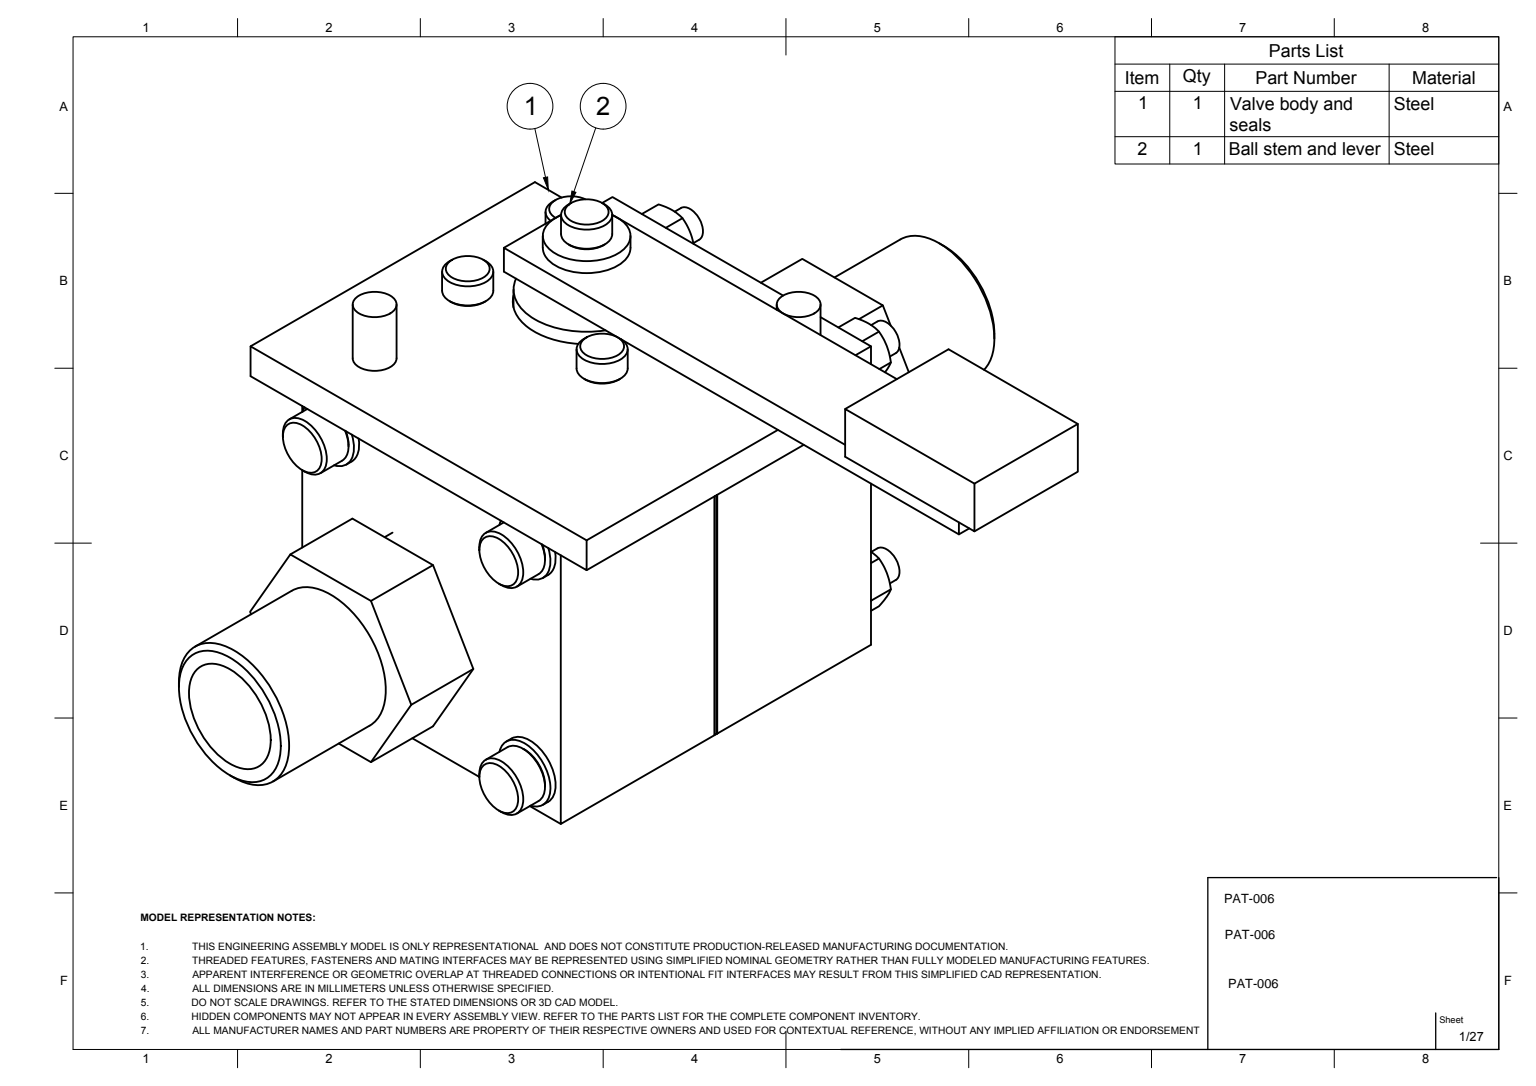
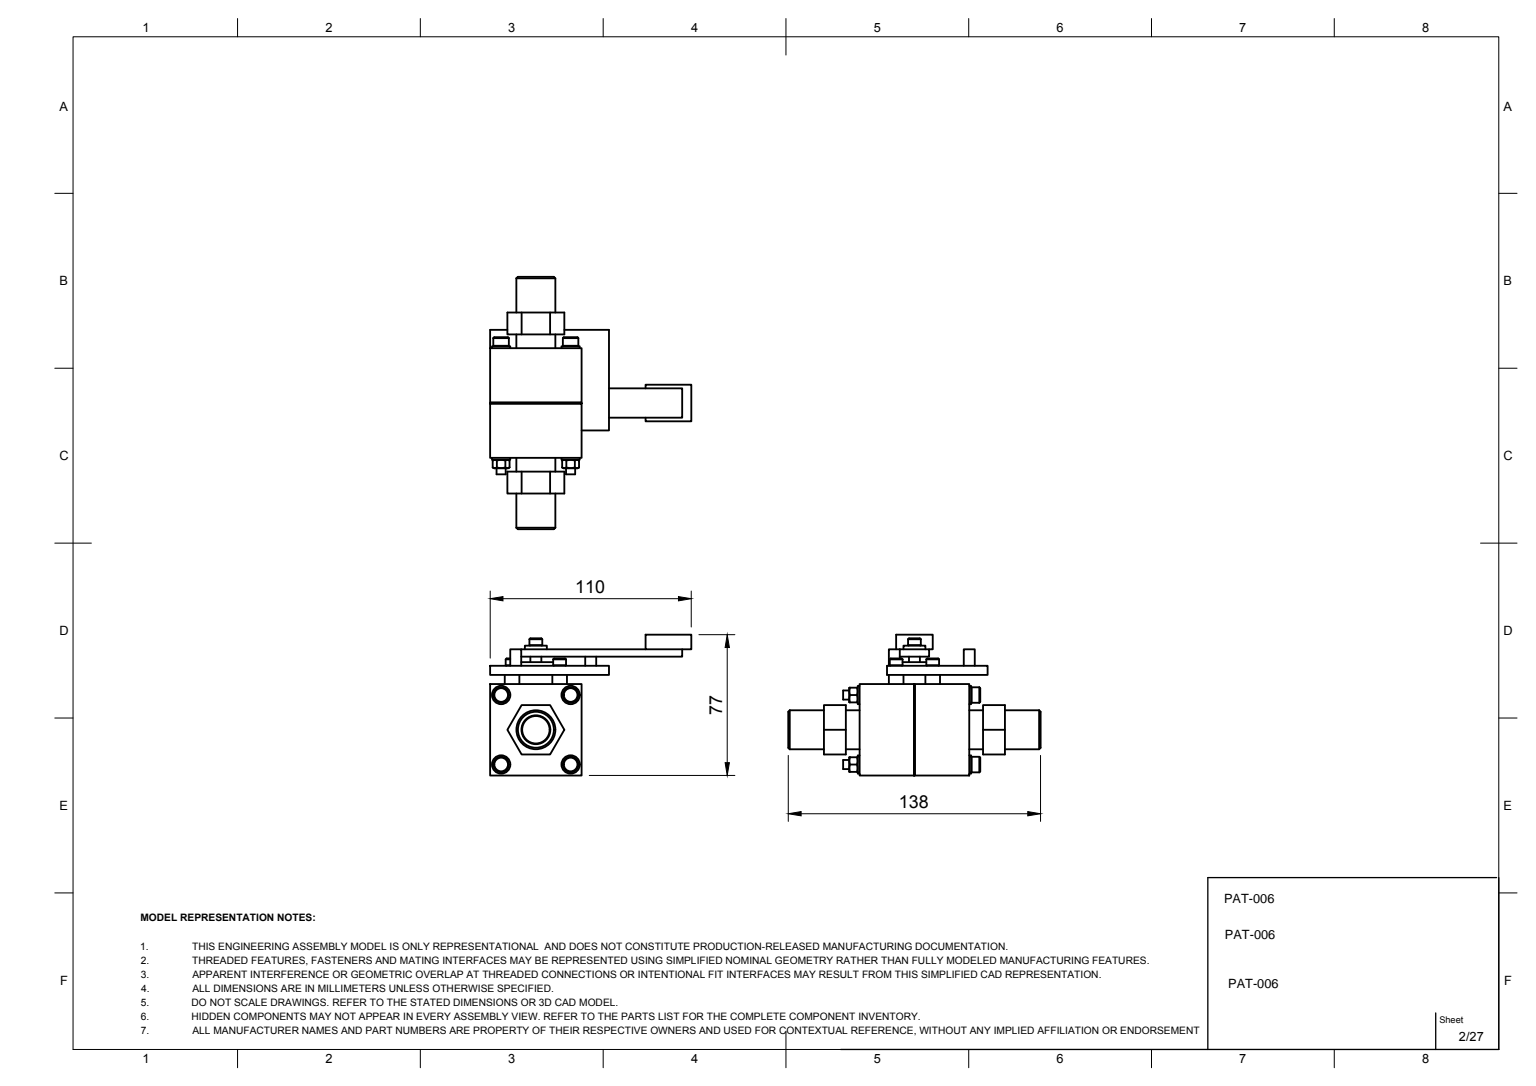
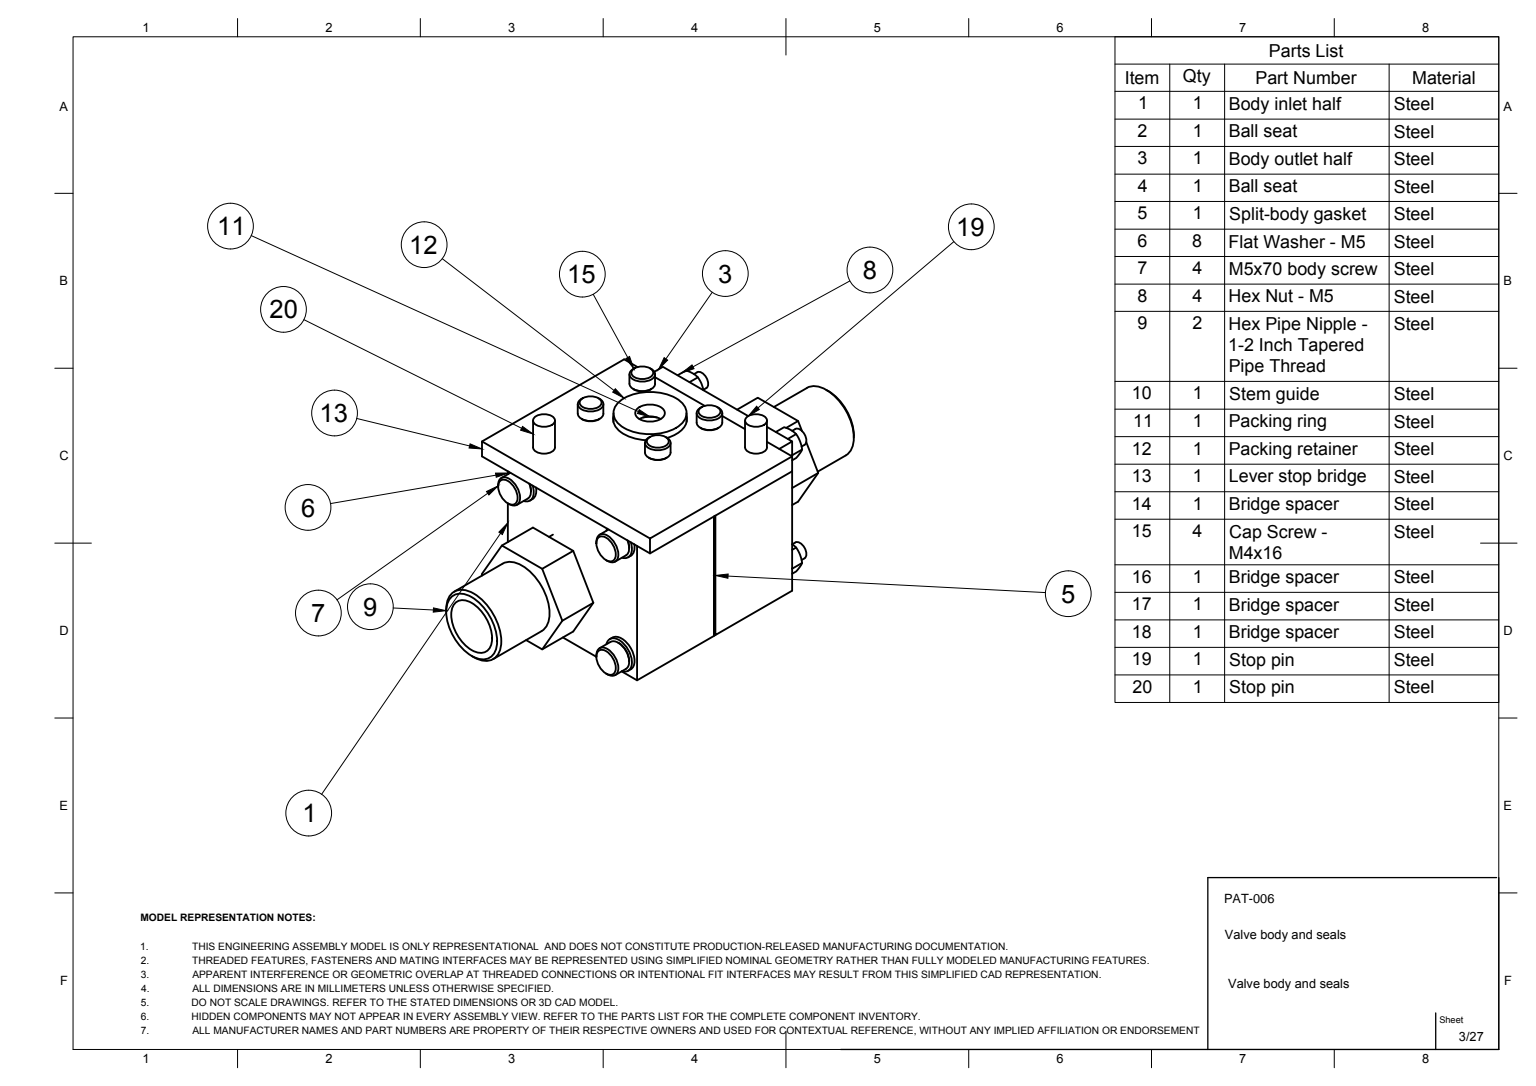
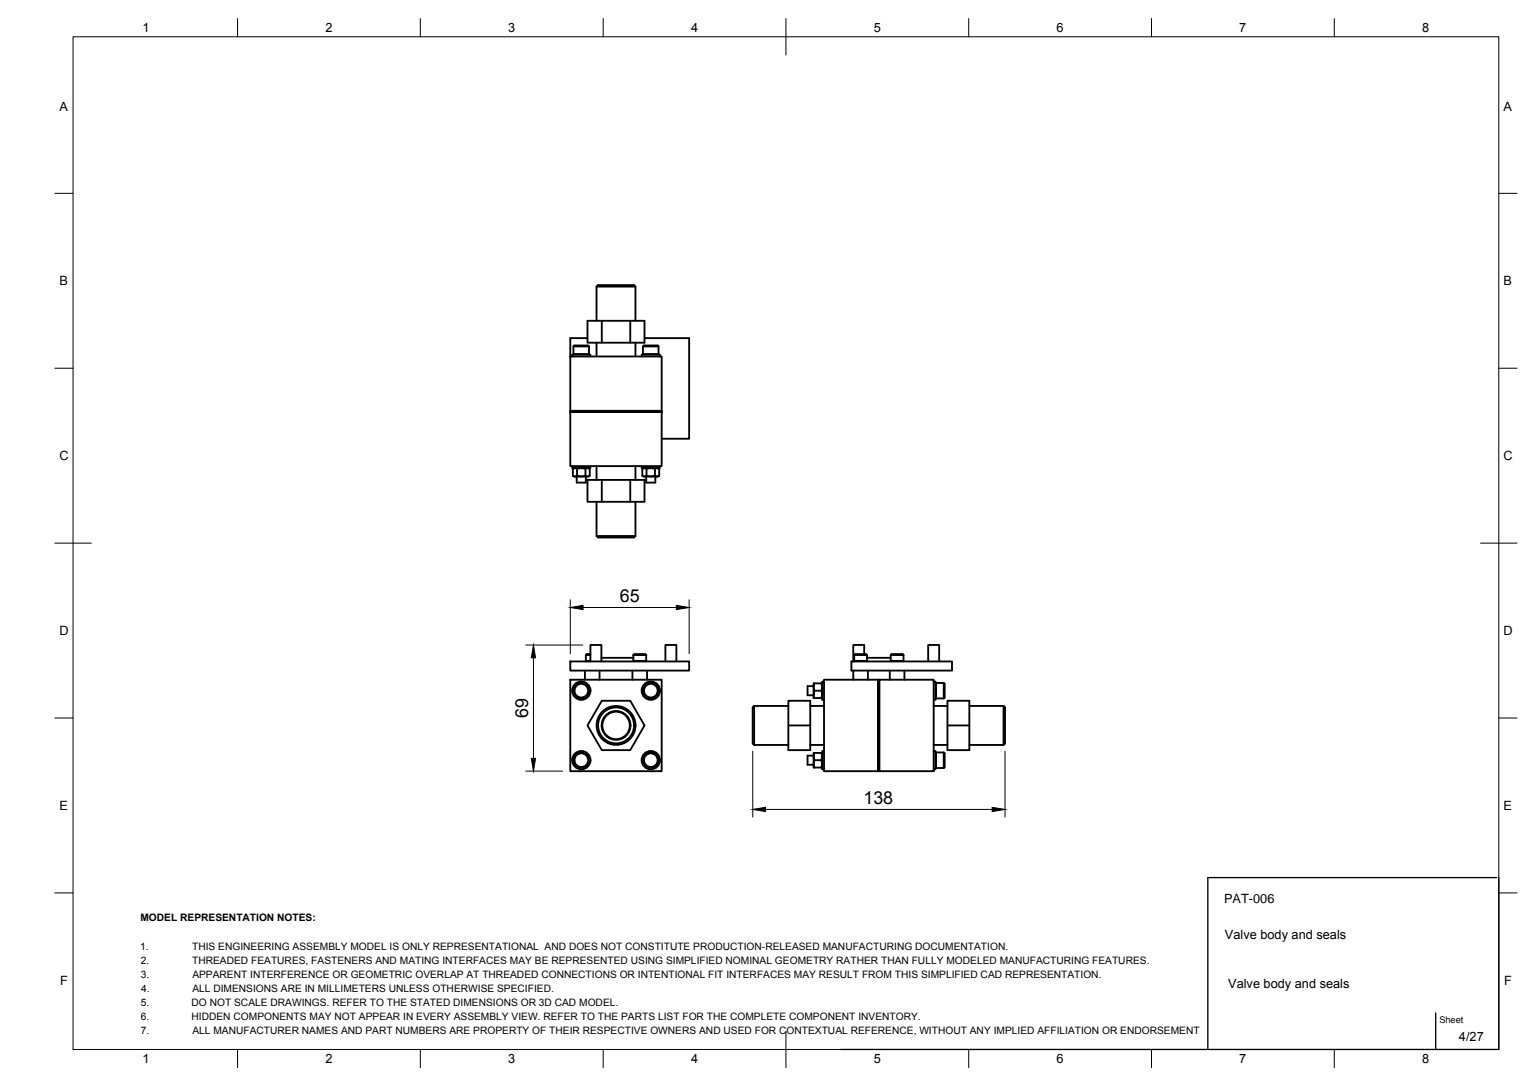
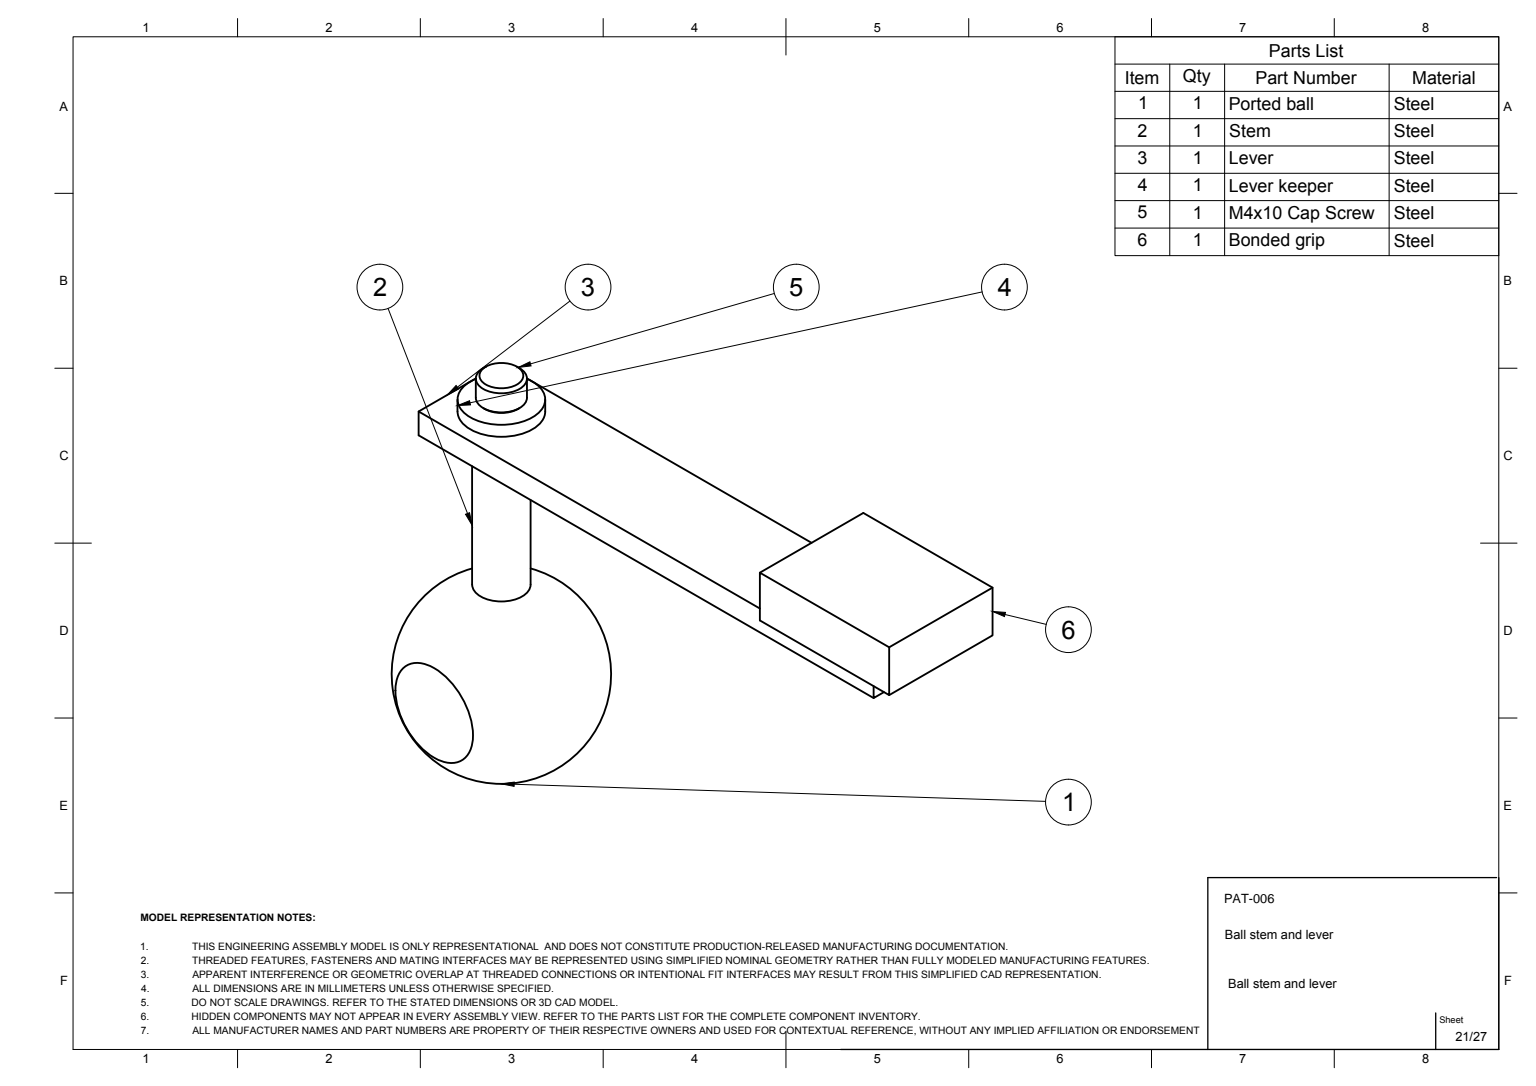
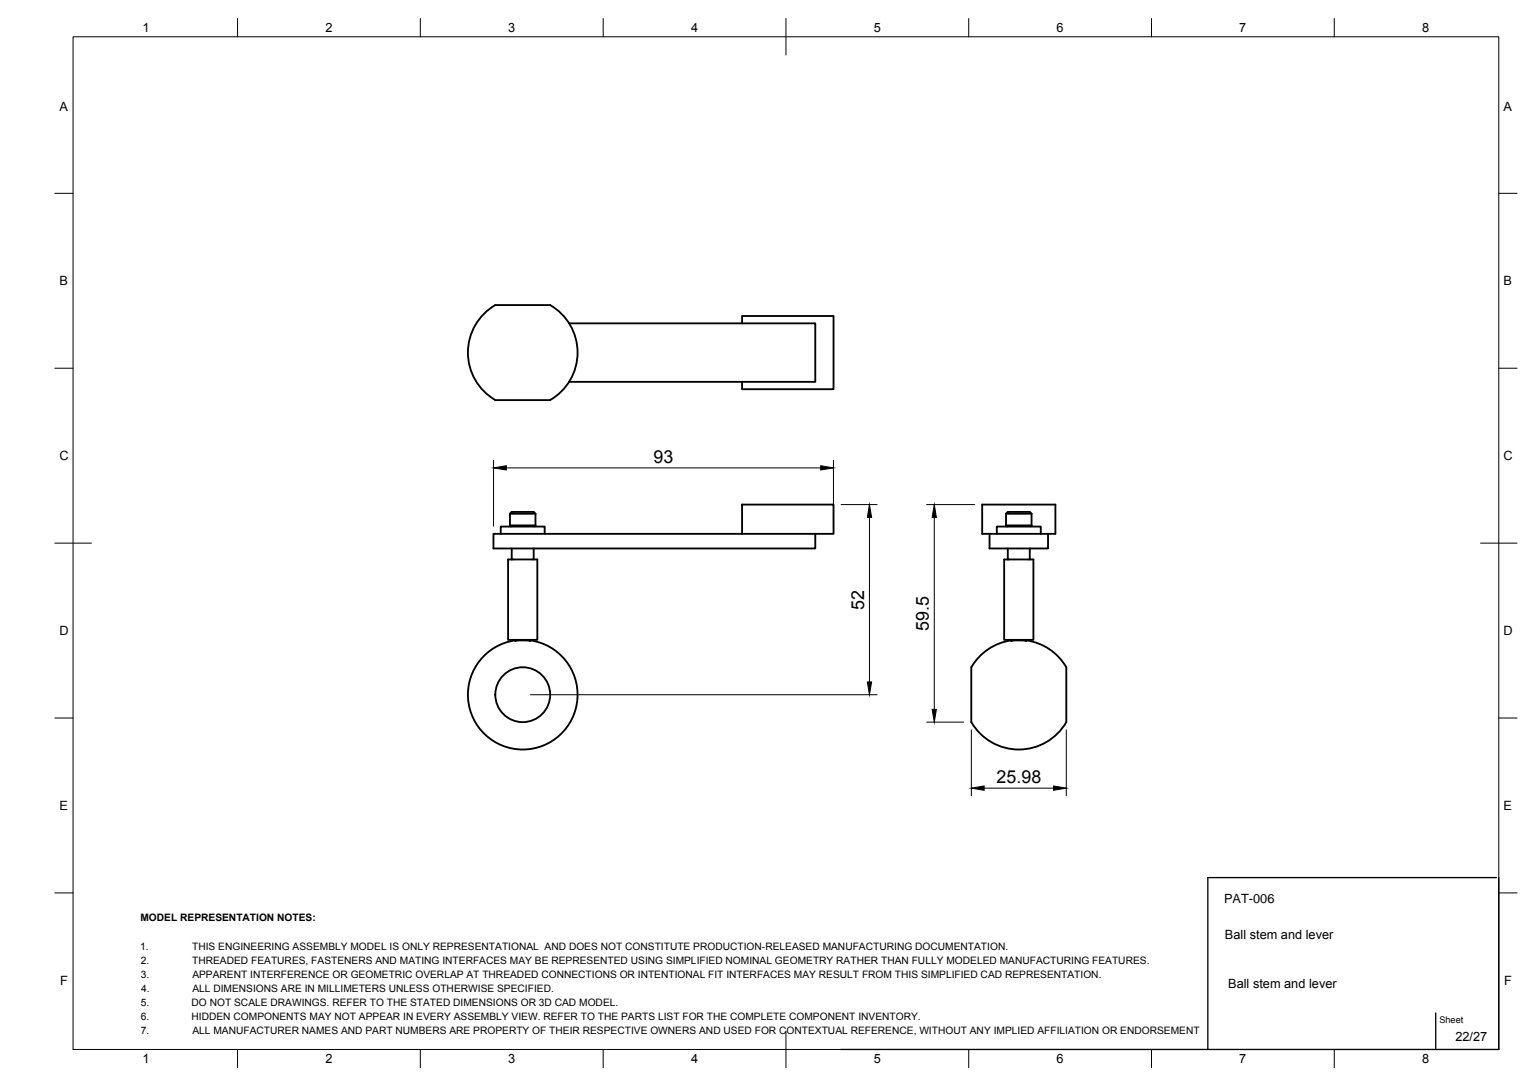
ISO-10303-21;
HEADER;
/* Generated by software containing ST-Developer
 * from STEP Tools, Inc. (www.steptools.com) 
 */

FILE_DESCRIPTION(
/* description */ ('Ball-type isolation valve (generic)'),
/* implementation_level */ '2;1');

FILE_NAME(
/* name */ 'PAT-006',
/* time_stamp */ '2026-10-27T10:53:05-07:00',
/* author */ (''),
/* organization */ (''),
/* preprocessor_version */ 'ST-DEVELOPER v20.2',
/* originating_system */ 'Autodesk Translation Framework v15.17.0.0',
/* authorisation */ '');

FILE_SCHEMA (('AUTOMOTIVE_DESIGN { 1 0 10303 214 3 1 1 }'));
ENDSEC;

DATA;
#10=MECHANICAL_DESIGN_GEOMETRIC_PRESENTATION_REPRESENTATION('',(#277,#278,
#279,#280,#281,#282,#283,#284,#285,#286,#287,#288,#289,#290,#291,#292,#293,
#294,#295,#296,#297,#298,#299,#300,#301,#302),#7425);
#11=ITEM_DEFINED_TRANSFORMATION($,$,#4400,#4748);
#12=ITEM_DEFINED_TRANSFORMATION($,$,#4443,#4749);
#13=ITEM_DEFINED_TRANSFORMATION($,$,#4454,#4750);
#14=ITEM_DEFINED_TRANSFORMATION($,$,#4497,#4751);
#15=ITEM_DEFINED_TRANSFORMATION($,$,#4508,#4752);
#16=ITEM_DEFINED_TRANSFORMATION($,$,#4535,#4753);
#17=ITEM_DEFINED_TRANSFORMATION($,$,#4548,#4754);
#18=ITEM_DEFINED_TRANSFORMATION($,$,#4552,#4755);
#19=ITEM_DEFINED_TRANSFORMATION($,$,#4565,#4756);
#20=ITEM_DEFINED_TRANSFORMATION($,$,#4595,#4757);
#21=ITEM_DEFINED_TRANSFORMATION($,$,#4604,#4758);
#22=ITEM_DEFINED_TRANSFORMATION($,$,#4613,#4759);
#23=ITEM_DEFINED_TRANSFORMATION($,$,#4622,#4760);
#24=ITEM_DEFINED_TRANSFORMATION($,$,#4631,#4761);
#25=ITEM_DEFINED_TRANSFORMATION($,$,#4637,#4762);
#26=ITEM_DEFINED_TRANSFORMATION($,$,#4671,#4763);
#27=ITEM_DEFINED_TRANSFORMATION($,$,#4643,#4764);
#28=ITEM_DEFINED_TRANSFORMATION($,$,#4671,#4765);
#29=ITEM_DEFINED_TRANSFORMATION($,$,#4682,#4766);
#30=ITEM_DEFINED_TRANSFORMATION($,$,#4671,#4767);
#31=ITEM_DEFINED_TRANSFORMATION($,$,#4643,#4768);
#32=ITEM_DEFINED_TRANSFORMATION($,$,#4671,#4769);
#33=ITEM_DEFINED_TRANSFORMATION($,$,#4682,#4770);
#34=ITEM_DEFINED_TRANSFORMATION($,$,#4671,#4771);
#35=ITEM_DEFINED_TRANSFORMATION($,$,#4643,#4772);
#36=ITEM_DEFINED_TRANSFORMATION($,$,#4671,#4773);
#37=ITEM_DEFINED_TRANSFORMATION($,$,#4682,#4774);
#38=ITEM_DEFINED_TRANSFORMATION($,$,#4671,#4775);
#39=ITEM_DEFINED_TRANSFORMATION($,$,#4643,#4776);
#40=ITEM_DEFINED_TRANSFORMATION($,$,#4671,#4777);
#41=ITEM_DEFINED_TRANSFORMATION($,$,#4682,#4778);
#42=ITEM_DEFINED_TRANSFORMATION($,$,#4698,#4779);
#43=ITEM_DEFINED_TRANSFORMATION($,$,#4698,#4780);
#44=ITEM_DEFINED_TRANSFORMATION($,$,#4722,#4781);
#45=ITEM_DEFINED_TRANSFORMATION($,$,#4722,#4782);
#46=ITEM_DEFINED_TRANSFORMATION($,$,#4722,#4783);
#47=ITEM_DEFINED_TRANSFORMATION($,$,#4722,#4784);
#48=ITEM_DEFINED_TRANSFORMATION($,$,#4786,#4888);
#49=ITEM_DEFINED_TRANSFORMATION($,$,#4802,#4889);
#50=ITEM_DEFINED_TRANSFORMATION($,$,#4837,#4890);
#51=ITEM_DEFINED_TRANSFORMATION($,$,#4848,#4891);
#52=ITEM_DEFINED_TRANSFORMATION($,$,#4857,#4892);
#53=ITEM_DEFINED_TRANSFORMATION($,$,#4864,#4893);
#54=ITEM_DEFINED_TRANSFORMATION($,$,#4399,#4894);
#55=ITEM_DEFINED_TRANSFORMATION($,$,#4785,#4895);
#56=(
REPRESENTATION_RELATIONSHIP($,$,#7535,#7534)
REPRESENTATION_RELATIONSHIP_WITH_TRANSFORMATION(#11)
SHAPE_REPRESENTATION_RELATIONSHIP()
);
#57=(
REPRESENTATION_RELATIONSHIP($,$,#7536,#7534)
REPRESENTATION_RELATIONSHIP_WITH_TRANSFORMATION(#12)
SHAPE_REPRESENTATION_RELATIONSHIP()
);
#58=(
REPRESENTATION_RELATIONSHIP($,$,#7537,#7534)
REPRESENTATION_RELATIONSHIP_WITH_TRANSFORMATION(#13)
SHAPE_REPRESENTATION_RELATIONSHIP()
);
#59=(
REPRESENTATION_RELATIONSHIP($,$,#7538,#7534)
REPRESENTATION_RELATIONSHIP_WITH_TRANSFORMATION(#14)
SHAPE_REPRESENTATION_RELATIONSHIP()
);
#60=(
REPRESENTATION_RELATIONSHIP($,$,#7539,#7534)
REPRESENTATION_RELATIONSHIP_WITH_TRANSFORMATION(#15)
SHAPE_REPRESENTATION_RELATIONSHIP()
);
#61=(
REPRESENTATION_RELATIONSHIP($,$,#7540,#7534)
REPRESENTATION_RELATIONSHIP_WITH_TRANSFORMATION(#16)
SHAPE_REPRESENTATION_RELATIONSHIP()
);
#62=(
REPRESENTATION_RELATIONSHIP($,$,#7541,#7534)
REPRESENTATION_RELATIONSHIP_WITH_TRANSFORMATION(#17)
SHAPE_REPRESENTATION_RELATIONSHIP()
);
#63=(
REPRESENTATION_RELATIONSHIP($,$,#7542,#7534)
REPRESENTATION_RELATIONSHIP_WITH_TRANSFORMATION(#18)
SHAPE_REPRESENTATION_RELATIONSHIP()
);
#64=(
REPRESENTATION_RELATIONSHIP($,$,#7543,#7534)
REPRESENTATION_RELATIONSHIP_WITH_TRANSFORMATION(#19)
SHAPE_REPRESENTATION_RELATIONSHIP()
);
#65=(
REPRESENTATION_RELATIONSHIP($,$,#7544,#7534)
REPRESENTATION_RELATIONSHIP_WITH_TRANSFORMATION(#20)
SHAPE_REPRESENTATION_RELATIONSHIP()
);
#66=(
REPRESENTATION_RELATIONSHIP($,$,#7545,#7534)
REPRESENTATION_RELATIONSHIP_WITH_TRANSFORMATION(#21)
SHAPE_REPRESENTATION_RELATIONSHIP()
);
#67=(
REPRESENTATION_RELATIONSHIP($,$,#7546,#7534)
REPRESENTATION_RELATIONSHIP_WITH_TRANSFORMATION(#22)
SHAPE_REPRESENTATION_RELATIONSHIP()
);
#68=(
REPRESENTATION_RELATIONSHIP($,$,#7547,#7534)
REPRESENTATION_RELATIONSHIP_WITH_TRANSFORMATION(#23)
SHAPE_REPRESENTATION_RELATIONSHIP()
);
#69=(
REPRESENTATION_RELATIONSHIP($,$,#7548,#7534)
REPRESENTATION_RELATIONSHIP_WITH_TRANSFORMATION(#24)
SHAPE_REPRESENTATION_RELATIONSHIP()
);
#70=(
REPRESENTATION_RELATIONSHIP($,$,#7549,#7534)
REPRESENTATION_RELATIONSHIP_WITH_TRANSFORMATION(#25)
SHAPE_REPRESENTATION_RELATIONSHIP()
);
#71=(
REPRESENTATION_RELATIONSHIP($,$,#7551,#7534)
REPRESENTATION_RELATIONSHIP_WITH_TRANSFORMATION(#26)
SHAPE_REPRESENTATION_RELATIONSHIP()
);
#72=(
REPRESENTATION_RELATIONSHIP($,$,#7550,#7534)
REPRESENTATION_RELATIONSHIP_WITH_TRANSFORMATION(#27)
SHAPE_REPRESENTATION_RELATIONSHIP()
);
#73=(
REPRESENTATION_RELATIONSHIP($,$,#7551,#7534)
REPRESENTATION_RELATIONSHIP_WITH_TRANSFORMATION(#28)
SHAPE_REPRESENTATION_RELATIONSHIP()
);
#74=(
REPRESENTATION_RELATIONSHIP($,$,#7552,#7534)
REPRESENTATION_RELATIONSHIP_WITH_TRANSFORMATION(#29)
SHAPE_REPRESENTATION_RELATIONSHIP()
);
#75=(
REPRESENTATION_RELATIONSHIP($,$,#7551,#7534)
REPRESENTATION_RELATIONSHIP_WITH_TRANSFORMATION(#30)
SHAPE_REPRESENTATION_RELATIONSHIP()
);
#76=(
REPRESENTATION_RELATIONSHIP($,$,#7550,#7534)
REPRESENTATION_RELATIONSHIP_WITH_TRANSFORMATION(#31)
SHAPE_REPRESENTATION_RELATIONSHIP()
);
#77=(
REPRESENTATION_RELATIONSHIP($,$,#7551,#7534)
REPRESENTATION_RELATIONSHIP_WITH_TRANSFORMATION(#32)
SHAPE_REPRESENTATION_RELATIONSHIP()
);
#78=(
REPRESENTATION_RELATIONSHIP($,$,#7552,#7534)
REPRESENTATION_RELATIONSHIP_WITH_TRANSFORMATION(#33)
SHAPE_REPRESENTATION_RELATIONSHIP()
);
#79=(
REPRESENTATION_RELATIONSHIP($,$,#7551,#7534)
REPRESENTATION_RELATIONSHIP_WITH_TRANSFORMATION(#34)
SHAPE_REPRESENTATION_RELATIONSHIP()
);
#80=(
REPRESENTATION_RELATIONSHIP($,$,#7550,#7534)
REPRESENTATION_RELATIONSHIP_WITH_TRANSFORMATION(#35)
SHAPE_REPRESENTATION_RELATIONSHIP()
);
#81=(
REPRESENTATION_RELATIONSHIP($,$,#7551,#7534)
REPRESENTATION_RELATIONSHIP_WITH_TRANSFORMATION(#36)
SHAPE_REPRESENTATION_RELATIONSHIP()
);
#82=(
REPRESENTATION_RELATIONSHIP($,$,#7552,#7534)
REPRESENTATION_RELATIONSHIP_WITH_TRANSFORMATION(#37)
SHAPE_REPRESENTATION_RELATIONSHIP()
);
#83=(
REPRESENTATION_RELATIONSHIP($,$,#7551,#7534)
REPRESENTATION_RELATIONSHIP_WITH_TRANSFORMATION(#38)
SHAPE_REPRESENTATION_RELATIONSHIP()
);
#84=(
REPRESENTATION_RELATIONSHIP($,$,#7550,#7534)
REPRESENTATION_RELATIONSHIP_WITH_TRANSFORMATION(#39)
SHAPE_REPRESENTATION_RELATIONSHIP()
);
#85=(
REPRESENTATION_RELATIONSHIP($,$,#7551,#7534)
REPRESENTATION_RELATIONSHIP_WITH_TRANSFORMATION(#40)
SHAPE_REPRESENTATION_RELATIONSHIP()
);
#86=(
REPRESENTATION_RELATIONSHIP($,$,#7552,#7534)
REPRESENTATION_RELATIONSHIP_WITH_TRANSFORMATION(#41)
SHAPE_REPRESENTATION_RELATIONSHIP()
);
#87=(
REPRESENTATION_RELATIONSHIP($,$,#7553,#7534)
REPRESENTATION_RELATIONSHIP_WITH_TRANSFORMATION(#42)
SHAPE_REPRESENTATION_RELATIONSHIP()
);
#88=(
REPRESENTATION_RELATIONSHIP($,$,#7553,#7534)
REPRESENTATION_RELATIONSHIP_WITH_TRANSFORMATION(#43)
SHAPE_REPRESENTATION_RELATIONSHIP()
);
#89=(
REPRESENTATION_RELATIONSHIP($,$,#7554,#7534)
REPRESENTATION_RELATIONSHIP_WITH_TRANSFORMATION(#44)
SHAPE_REPRESENTATION_RELATIONSHIP()
);
#90=(
REPRESENTATION_RELATIONSHIP($,$,#7554,#7534)
REPRESENTATION_RELATIONSHIP_WITH_TRANSFORMATION(#45)
SHAPE_REPRESENTATION_RELATIONSHIP()
);
#91=(
REPRESENTATION_RELATIONSHIP($,$,#7554,#7534)
REPRESENTATION_RELATIONSHIP_WITH_TRANSFORMATION(#46)
SHAPE_REPRESENTATION_RELATIONSHIP()
);
#92=(
REPRESENTATION_RELATIONSHIP($,$,#7554,#7534)
REPRESENTATION_RELATIONSHIP_WITH_TRANSFORMATION(#47)
SHAPE_REPRESENTATION_RELATIONSHIP()
);
#93=(
REPRESENTATION_RELATIONSHIP($,$,#7556,#7555)
REPRESENTATION_RELATIONSHIP_WITH_TRANSFORMATION(#48)
SHAPE_REPRESENTATION_RELATIONSHIP()
);
#94=(
REPRESENTATION_RELATIONSHIP($,$,#7557,#7555)
REPRESENTATION_RELATIONSHIP_WITH_TRANSFORMATION(#49)
SHAPE_REPRESENTATION_RELATIONSHIP()
);
#95=(
REPRESENTATION_RELATIONSHIP($,$,#7558,#7555)
REPRESENTATION_RELATIONSHIP_WITH_TRANSFORMATION(#50)
SHAPE_REPRESENTATION_RELATIONSHIP()
);
#96=(
REPRESENTATION_RELATIONSHIP($,$,#7559,#7555)
REPRESENTATION_RELATIONSHIP_WITH_TRANSFORMATION(#51)
SHAPE_REPRESENTATION_RELATIONSHIP()
);
#97=(
REPRESENTATION_RELATIONSHIP($,$,#7560,#7555)
REPRESENTATION_RELATIONSHIP_WITH_TRANSFORMATION(#52)
SHAPE_REPRESENTATION_RELATIONSHIP()
);
#98=(
REPRESENTATION_RELATIONSHIP($,$,#7561,#7555)
REPRESENTATION_RELATIONSHIP_WITH_TRANSFORMATION(#53)
SHAPE_REPRESENTATION_RELATIONSHIP()
);
#99=(
REPRESENTATION_RELATIONSHIP($,$,#7534,#7533)
REPRESENTATION_RELATIONSHIP_WITH_TRANSFORMATION(#54)
SHAPE_REPRESENTATION_RELATIONSHIP()
);
#100=(
REPRESENTATION_RELATIONSHIP($,$,#7555,#7533)
REPRESENTATION_RELATIONSHIP_WITH_TRANSFORMATION(#55)
SHAPE_REPRESENTATION_RELATIONSHIP()
);
#101=CONTEXT_DEPENDENT_SHAPE_REPRESENTATION(#56,#7481);
#102=CONTEXT_DEPENDENT_SHAPE_REPRESENTATION(#57,#7482);
#103=CONTEXT_DEPENDENT_SHAPE_REPRESENTATION(#58,#7483);
#104=CONTEXT_DEPENDENT_SHAPE_REPRESENTATION(#59,#7484);
#105=CONTEXT_DEPENDENT_SHAPE_REPRESENTATION(#60,#7485);
#106=CONTEXT_DEPENDENT_SHAPE_REPRESENTATION(#61,#7486);
#107=CONTEXT_DEPENDENT_SHAPE_REPRESENTATION(#62,#7487);
#108=CONTEXT_DEPENDENT_SHAPE_REPRESENTATION(#63,#7488);
#109=CONTEXT_DEPENDENT_SHAPE_REPRESENTATION(#64,#7489);
#110=CONTEXT_DEPENDENT_SHAPE_REPRESENTATION(#65,#7490);
#111=CONTEXT_DEPENDENT_SHAPE_REPRESENTATION(#66,#7491);
#112=CONTEXT_DEPENDENT_SHAPE_REPRESENTATION(#67,#7492);
#113=CONTEXT_DEPENDENT_SHAPE_REPRESENTATION(#68,#7493);
#114=CONTEXT_DEPENDENT_SHAPE_REPRESENTATION(#69,#7494);
#115=CONTEXT_DEPENDENT_SHAPE_REPRESENTATION(#70,#7495);
#116=CONTEXT_DEPENDENT_SHAPE_REPRESENTATION(#71,#7496);
#117=CONTEXT_DEPENDENT_SHAPE_REPRESENTATION(#72,#7497);
#118=CONTEXT_DEPENDENT_SHAPE_REPRESENTATION(#73,#7498);
#119=CONTEXT_DEPENDENT_SHAPE_REPRESENTATION(#74,#7499);
#120=CONTEXT_DEPENDENT_SHAPE_REPRESENTATION(#75,#7500);
#121=CONTEXT_DEPENDENT_SHAPE_REPRESENTATION(#76,#7501);
#122=CONTEXT_DEPENDENT_SHAPE_REPRESENTATION(#77,#7502);
#123=CONTEXT_DEPENDENT_SHAPE_REPRESENTATION(#78,#7503);
#124=CONTEXT_DEPENDENT_SHAPE_REPRESENTATION(#79,#7504);
#125=CONTEXT_DEPENDENT_SHAPE_REPRESENTATION(#80,#7505);
#126=CONTEXT_DEPENDENT_SHAPE_REPRESENTATION(#81,#7506);
#127=CONTEXT_DEPENDENT_SHAPE_REPRESENTATION(#82,#7507);
#128=CONTEXT_DEPENDENT_SHAPE_REPRESENTATION(#83,#7508);
#129=CONTEXT_DEPENDENT_SHAPE_REPRESENTATION(#84,#7509);
#130=CONTEXT_DEPENDENT_SHAPE_REPRESENTATION(#85,#7510);
#131=CONTEXT_DEPENDENT_SHAPE_REPRESENTATION(#86,#7511);
#132=CONTEXT_DEPENDENT_SHAPE_REPRESENTATION(#87,#7512);
#133=CONTEXT_DEPENDENT_SHAPE_REPRESENTATION(#88,#7513);
#134=CONTEXT_DEPENDENT_SHAPE_REPRESENTATION(#89,#7514);
#135=CONTEXT_DEPENDENT_SHAPE_REPRESENTATION(#90,#7515);
#136=CONTEXT_DEPENDENT_SHAPE_REPRESENTATION(#91,#7516);
#137=CONTEXT_DEPENDENT_SHAPE_REPRESENTATION(#92,#7517);
#138=CONTEXT_DEPENDENT_SHAPE_REPRESENTATION(#93,#7525);
#139=CONTEXT_DEPENDENT_SHAPE_REPRESENTATION(#94,#7526);
#140=CONTEXT_DEPENDENT_SHAPE_REPRESENTATION(#95,#7527);
#141=CONTEXT_DEPENDENT_SHAPE_REPRESENTATION(#96,#7528);
#142=CONTEXT_DEPENDENT_SHAPE_REPRESENTATION(#97,#7529);
#143=CONTEXT_DEPENDENT_SHAPE_REPRESENTATION(#98,#7530);
#144=CONTEXT_DEPENDENT_SHAPE_REPRESENTATION(#99,#7531);
#145=CONTEXT_DEPENDENT_SHAPE_REPRESENTATION(#100,#7532);
#146=NEXT_ASSEMBLY_USAGE_OCCURRENCE('Body inlet half:1',
'Body inlet half:1','Body inlet half:1',#7564,#7565,'Body inlet half:1');
#147=NEXT_ASSEMBLY_USAGE_OCCURRENCE('Ball seat:1','Ball seat:1',
'Ball seat:1',#7564,#7566,'Ball seat:1');
#148=NEXT_ASSEMBLY_USAGE_OCCURRENCE('Body outlet half:1',
'Body outlet half:1','Body outlet half:1',#7564,#7567,
'Body outlet half:1');
#149=NEXT_ASSEMBLY_USAGE_OCCURRENCE('Ball seat (1):1','Ball seat (1):1',
'Ball seat (1):1',#7564,#7568,'Ball seat (1):1');
#150=NEXT_ASSEMBLY_USAGE_OCCURRENCE('Split-body gasket:1',
'Split-body gasket:1','Split-body gasket:1',#7564,#7569,
'Split-body gasket:1');
#151=NEXT_ASSEMBLY_USAGE_OCCURRENCE('Stem guide:1','Stem guide:1',
'Stem guide:1',#7564,#7570,'Stem guide:1');
#152=NEXT_ASSEMBLY_USAGE_OCCURRENCE('Packing ring:1','Packing ring:1',
'Packing ring:1',#7564,#7571,'Packing ring:1');
#153=NEXT_ASSEMBLY_USAGE_OCCURRENCE('Packing retainer:1',
'Packing retainer:1','Packing retainer:1',#7564,#7572,
'Packing retainer:1');
#154=NEXT_ASSEMBLY_USAGE_OCCURRENCE('Lever stop bridge:1',
'Lever stop bridge:1','Lever stop bridge:1',#7564,#7573,
'Lever stop bridge:1');
#155=NEXT_ASSEMBLY_USAGE_OCCURRENCE('Bridge spacer:1','Bridge spacer:1',
'Bridge spacer:1',#7564,#7574,'Bridge spacer:1');
#156=NEXT_ASSEMBLY_USAGE_OCCURRENCE('Bridge spacer (1):1',
'Bridge spacer (1):1','Bridge spacer (1):1',#7564,#7575,
'Bridge spacer (1):1');
#157=NEXT_ASSEMBLY_USAGE_OCCURRENCE('Bridge spacer (2):1',
'Bridge spacer (2):1','Bridge spacer (2):1',#7564,#7576,
'Bridge spacer (2):1');
#158=NEXT_ASSEMBLY_USAGE_OCCURRENCE('Bridge spacer (3):1',
'Bridge spacer (3):1','Bridge spacer (3):1',#7564,#7577,
'Bridge spacer (3):1');
#159=NEXT_ASSEMBLY_USAGE_OCCURRENCE('Stop pin:1','Stop pin:1',
'Stop pin:1',#7564,#7578,'Stop pin:1');
#160=NEXT_ASSEMBLY_USAGE_OCCURRENCE('Stop pin (1):1','Stop pin (1):1',
'Stop pin (1):1',#7564,#7579,'Stop pin (1):1');
#161=NEXT_ASSEMBLY_USAGE_OCCURRENCE('Flat Washer - M5:2',
'Flat Washer - M5:2','Flat Washer - M5:2',#7564,#7581,
'Flat Washer - M5:2');
#162=NEXT_ASSEMBLY_USAGE_OCCURRENCE('M5x70 body screw:2',
'M5x70 body screw:2','M5x70 body screw:2',#7564,#7580,
'M5x70 body screw:2');
#163=NEXT_ASSEMBLY_USAGE_OCCURRENCE('Flat Washer - M5:3',
'Flat Washer - M5:3','Flat Washer - M5:3',#7564,#7581,
'Flat Washer - M5:3');
#164=NEXT_ASSEMBLY_USAGE_OCCURRENCE('Hex Nut - M5:2','Hex Nut - M5:2',
'Hex Nut - M5:2',#7564,#7582,'Hex Nut - M5:2');
#165=NEXT_ASSEMBLY_USAGE_OCCURRENCE('Flat Washer - M5:4',
'Flat Washer - M5:4','Flat Washer - M5:4',#7564,#7581,
'Flat Washer - M5:4');
#166=NEXT_ASSEMBLY_USAGE_OCCURRENCE('M5x70 body screw:3',
'M5x70 body screw:3','M5x70 body screw:3',#7564,#7580,
'M5x70 body screw:3');
#167=NEXT_ASSEMBLY_USAGE_OCCURRENCE('Flat Washer - M5:5',
'Flat Washer - M5:5','Flat Washer - M5:5',#7564,#7581,
'Flat Washer - M5:5');
#168=NEXT_ASSEMBLY_USAGE_OCCURRENCE('Hex Nut - M5:3','Hex Nut - M5:3',
'Hex Nut - M5:3',#7564,#7582,'Hex Nut - M5:3');
#169=NEXT_ASSEMBLY_USAGE_OCCURRENCE('Flat Washer - M5:6',
'Flat Washer - M5:6','Flat Washer - M5:6',#7564,#7581,
'Flat Washer - M5:6');
#170=NEXT_ASSEMBLY_USAGE_OCCURRENCE('M5x70 body screw:4',
'M5x70 body screw:4','M5x70 body screw:4',#7564,#7580,
'M5x70 body screw:4');
#171=NEXT_ASSEMBLY_USAGE_OCCURRENCE('Flat Washer - M5:7',
'Flat Washer - M5:7','Flat Washer - M5:7',#7564,#7581,
'Flat Washer - M5:7');
#172=NEXT_ASSEMBLY_USAGE_OCCURRENCE('Hex Nut - M5:4','Hex Nut - M5:4',
'Hex Nut - M5:4',#7564,#7582,'Hex Nut - M5:4');
#173=NEXT_ASSEMBLY_USAGE_OCCURRENCE('Flat Washer - M5:8',
'Flat Washer - M5:8','Flat Washer - M5:8',#7564,#7581,
'Flat Washer - M5:8');
#174=NEXT_ASSEMBLY_USAGE_OCCURRENCE('M5x70 body screw:5',
'M5x70 body screw:5','M5x70 body screw:5',#7564,#7580,
'M5x70 body screw:5');
#175=NEXT_ASSEMBLY_USAGE_OCCURRENCE('Flat Washer - M5:9',
'Flat Washer - M5:9','Flat Washer - M5:9',#7564,#7581,
'Flat Washer - M5:9');
#176=NEXT_ASSEMBLY_USAGE_OCCURRENCE('Hex Nut - M5:5','Hex Nut - M5:5',
'Hex Nut - M5:5',#7564,#7582,'Hex Nut - M5:5');
#177=NEXT_ASSEMBLY_USAGE_OCCURRENCE(
'Hex Pipe Nipple - 1-2 Inch Tapered Pipe Thread:2',
'Hex Pipe Nipple - 1-2 Inch Tapered Pipe Thread:2',
'Hex Pipe Nipple - 1-2 Inch Tapered Pipe Thread:2',#7564,#7583,
'Hex Pipe Nipple - 1-2 Inch Tapered Pipe Thread:2');
#178=NEXT_ASSEMBLY_USAGE_OCCURRENCE(
'Hex Pipe Nipple - 1-2 Inch Tapered Pipe Thread:3',
'Hex Pipe Nipple - 1-2 Inch Tapered Pipe Thread:3',
'Hex Pipe Nipple - 1-2 Inch Tapered Pipe Thread:3',#7564,#7583,
'Hex Pipe Nipple - 1-2 Inch Tapered Pipe Thread:3');
#179=NEXT_ASSEMBLY_USAGE_OCCURRENCE('Cap Screw - M4x16:2',
'Cap Screw - M4x16:2','Cap Screw - M4x16:2',#7564,#7584,
'Cap Screw - M4x16:2');
#180=NEXT_ASSEMBLY_USAGE_OCCURRENCE('Cap Screw - M4x16:3',
'Cap Screw - M4x16:3','Cap Screw - M4x16:3',#7564,#7584,
'Cap Screw - M4x16:3');
#181=NEXT_ASSEMBLY_USAGE_OCCURRENCE('Cap Screw - M4x16:4',
'Cap Screw - M4x16:4','Cap Screw - M4x16:4',#7564,#7584,
'Cap Screw - M4x16:4');
#182=NEXT_ASSEMBLY_USAGE_OCCURRENCE('Cap Screw - M4x16:5',
'Cap Screw - M4x16:5','Cap Screw - M4x16:5',#7564,#7584,
'Cap Screw - M4x16:5');
#183=NEXT_ASSEMBLY_USAGE_OCCURRENCE('Ported ball:1','Ported ball:1',
'Ported ball:1',#7585,#7586,'Ported ball:1');
#184=NEXT_ASSEMBLY_USAGE_OCCURRENCE('Stem:1','Stem:1','Stem:1',#7585,#7587,
'Stem:1');
#185=NEXT_ASSEMBLY_USAGE_OCCURRENCE('Lever:1','Lever:1','Lever:1',#7585,
#7588,'Lever:1');
#186=NEXT_ASSEMBLY_USAGE_OCCURRENCE('Lever keeper:1','Lever keeper:1',
'Lever keeper:1',#7585,#7589,'Lever keeper:1');
#187=NEXT_ASSEMBLY_USAGE_OCCURRENCE('Bonded grip:1','Bonded grip:1',
'Bonded grip:1',#7585,#7590,'Bonded grip:1');
#188=NEXT_ASSEMBLY_USAGE_OCCURRENCE('M4x10 Cap Screw:2',
'M4x10 Cap Screw:2','M4x10 Cap Screw:2',#7585,#7591,'M4x10 Cap Screw:2');
#189=NEXT_ASSEMBLY_USAGE_OCCURRENCE('Valve body and seals:1',
'Valve body and seals:1','Valve body and seals:1',#7563,#7564,
'Valve body and seals:1');
#190=NEXT_ASSEMBLY_USAGE_OCCURRENCE('Ball stem and lever:1',
'Ball stem and lever:1','Ball stem and lever:1',#7563,#7585,
'Ball stem and lever:1');
#191=(
BOUNDED_CURVE()
B_SPLINE_CURVE(2,(#6817,#6818,#6819),.UNSPECIFIED.,.F.,.F.)
B_SPLINE_CURVE_WITH_KNOTS((3,3),(0.140651836354967,0.670383167684795),
 .UNSPECIFIED.)
CURVE()
GEOMETRIC_REPRESENTATION_ITEM()
RATIONAL_B_SPLINE_CURVE((1.11602540378444,1.28867513459481,1.11602540378444))
REPRESENTATION_ITEM('')
);
#192=(
BOUNDED_CURVE()
B_SPLINE_CURVE(2,(#6821,#6822,#6823),.UNSPECIFIED.,.F.,.F.)
B_SPLINE_CURVE_WITH_KNOTS((3,3),(0.140651836354967,0.670383167684795),
 .UNSPECIFIED.)
CURVE()
GEOMETRIC_REPRESENTATION_ITEM()
RATIONAL_B_SPLINE_CURVE((1.11602540378444,1.28867513459481,1.11602540378444))
REPRESENTATION_ITEM('')
);
#193=(
BOUNDED_CURVE()
B_SPLINE_CURVE(2,(#6828,#6829,#6830),.UNSPECIFIED.,.F.,.F.)
B_SPLINE_CURVE_WITH_KNOTS((3,3),(0.140651836354967,0.670383167684795),
 .UNSPECIFIED.)
CURVE()
GEOMETRIC_REPRESENTATION_ITEM()
RATIONAL_B_SPLINE_CURVE((1.11602540378444,1.28867513459481,1.11602540378444))
REPRESENTATION_ITEM('')
);
#194=(
BOUNDED_CURVE()
B_SPLINE_CURVE(2,(#6832,#6833,#6834),.UNSPECIFIED.,.F.,.F.)
B_SPLINE_CURVE_WITH_KNOTS((3,3),(0.140651836354967,0.670383167684795),
 .UNSPECIFIED.)
CURVE()
GEOMETRIC_REPRESENTATION_ITEM()
RATIONAL_B_SPLINE_CURVE((1.11602540378444,1.28867513459481,1.11602540378444))
REPRESENTATION_ITEM('')
);
#195=(
BOUNDED_CURVE()
B_SPLINE_CURVE(2,(#6836,#6837,#6838),.UNSPECIFIED.,.F.,.F.)
B_SPLINE_CURVE_WITH_KNOTS((3,3),(0.140651836354967,0.670383167684795),
 .UNSPECIFIED.)
CURVE()
GEOMETRIC_REPRESENTATION_ITEM()
RATIONAL_B_SPLINE_CURVE((1.11602540378444,1.28867513459481,1.11602540378444))
REPRESENTATION_ITEM('')
);
#196=(
BOUNDED_CURVE()
B_SPLINE_CURVE(2,(#6839,#6840,#6841),.UNSPECIFIED.,.F.,.F.)
B_SPLINE_CURVE_WITH_KNOTS((3,3),(0.140651836354967,0.670383167684795),
 .UNSPECIFIED.)
CURVE()
GEOMETRIC_REPRESENTATION_ITEM()
RATIONAL_B_SPLINE_CURVE((1.11602540378444,1.28867513459481,1.11602540378444))
REPRESENTATION_ITEM('')
);
#197=(
BOUNDED_CURVE()
B_SPLINE_CURVE(2,(#6848,#6849,#6850),.UNSPECIFIED.,.F.,.F.)
B_SPLINE_CURVE_WITH_KNOTS((3,3),(0.140651836354967,0.670383167684795),
 .UNSPECIFIED.)
CURVE()
GEOMETRIC_REPRESENTATION_ITEM()
RATIONAL_B_SPLINE_CURVE((1.11602540378444,1.28867513459481,1.11602540378444))
REPRESENTATION_ITEM('')
);
#198=(
BOUNDED_CURVE()
B_SPLINE_CURVE(2,(#6852,#6853,#6854),.UNSPECIFIED.,.F.,.F.)
B_SPLINE_CURVE_WITH_KNOTS((3,3),(0.140651836354967,0.670383167684796),
 .UNSPECIFIED.)
CURVE()
GEOMETRIC_REPRESENTATION_ITEM()
RATIONAL_B_SPLINE_CURVE((1.11602540378444,1.28867513459481,1.11602540378444))
REPRESENTATION_ITEM('')
);
#199=(
BOUNDED_CURVE()
B_SPLINE_CURVE(2,(#6856,#6857,#6858),.UNSPECIFIED.,.F.,.F.)
B_SPLINE_CURVE_WITH_KNOTS((3,3),(0.140651836354967,0.670383167684795),
 .UNSPECIFIED.)
CURVE()
GEOMETRIC_REPRESENTATION_ITEM()
RATIONAL_B_SPLINE_CURVE((1.11602540378444,1.28867513459481,1.11602540378444))
REPRESENTATION_ITEM('')
);
#200=(
BOUNDED_CURVE()
B_SPLINE_CURVE(2,(#6860,#6861,#6862),.UNSPECIFIED.,.F.,.F.)
B_SPLINE_CURVE_WITH_KNOTS((3,3),(0.140651836354967,0.670383167684795),
 .UNSPECIFIED.)
CURVE()
GEOMETRIC_REPRESENTATION_ITEM()
RATIONAL_B_SPLINE_CURVE((1.11602540378444,1.28867513459482,1.11602540378444))
REPRESENTATION_ITEM('')
);
#201=(
BOUNDED_CURVE()
B_SPLINE_CURVE(2,(#6864,#6865,#6866),.UNSPECIFIED.,.F.,.F.)
B_SPLINE_CURVE_WITH_KNOTS((3,3),(0.140651836354967,0.670383167684795),
 .UNSPECIFIED.)
CURVE()
GEOMETRIC_REPRESENTATION_ITEM()
RATIONAL_B_SPLINE_CURVE((1.11602540378444,1.28867513459481,1.11602540378444))
REPRESENTATION_ITEM('')
);
#202=(
BOUNDED_CURVE()
B_SPLINE_CURVE(2,(#6867,#6868,#6869),.UNSPECIFIED.,.F.,.F.)
B_SPLINE_CURVE_WITH_KNOTS((3,3),(0.140651836354967,0.670383167684795),
 .UNSPECIFIED.)
CURVE()
GEOMETRIC_REPRESENTATION_ITEM()
RATIONAL_B_SPLINE_CURVE((1.11602540378444,1.28867513459481,1.11602540378444))
REPRESENTATION_ITEM('')
);
#203=CONICAL_SURFACE('',#4660,0.4,0.785398163397448);
#204=CONICAL_SURFACE('',#4664,0.41,0.785398163397448);
#205=CONICAL_SURFACE('',#4668,0.26,0.463647609000806);
#206=CONICAL_SURFACE('',#4672,0.275,0.785398163397449);
#207=CONICAL_SURFACE('',#4683,0.47094010767585,1.0471975511966);
#208=CONICAL_SURFACE('',#4685,0.47094010767585,1.0471975511966);
#209=CONICAL_SURFACE('',#4714,1.025,0.785398163397448);
#210=CONICAL_SURFACE('',#4717,1.025,0.785398163397448);
#211=CONICAL_SURFACE('',#4725,0.325,0.785398163397448);
#212=CONICAL_SURFACE('',#4729,0.335,0.785398163397448);
#213=CONICAL_SURFACE('',#4733,0.21,0.463647609000806);
#214=CONICAL_SURFACE('',#4737,0.18,0.785398163397448);
#215=CONICAL_SURFACE('',#4877,0.325,0.785398163397448);
#216=CONICAL_SURFACE('',#4881,0.335,0.785398163397448);
#217=CONICAL_SURFACE('',#4885,0.21,0.463647609000806);
#218=ORIENTED_CLOSED_SHELL('',*,#4097,.F.);
#219=ORIENTED_CLOSED_SHELL('',*,#4103,.F.);
#220=ORIENTED_CLOSED_SHELL('',*,#4109,.F.);
#221=BREP_WITH_VOIDS('Body1',#4098,(#218));
#222=BREP_WITH_VOIDS('Body1',#4102,(#219));
#223=BREP_WITH_VOIDS('Body1',#4110,(#220));
#224=TOROIDAL_SURFACE('',#4549,0.5,0.1);
#225=SHAPE_REPRESENTATION_RELATIONSHIP('SRR','None',#7535,#251);
#226=SHAPE_REPRESENTATION_RELATIONSHIP('SRR','None',#7536,#252);
#227=SHAPE_REPRESENTATION_RELATIONSHIP('SRR','None',#7537,#253);
#228=SHAPE_REPRESENTATION_RELATIONSHIP('SRR','None',#7538,#254);
#229=SHAPE_REPRESENTATION_RELATIONSHIP('SRR','None',#7539,#255);
#230=SHAPE_REPRESENTATION_RELATIONSHIP('SRR','None',#7540,#256);
#231=SHAPE_REPRESENTATION_RELATIONSHIP('SRR','None',#7541,#257);
#232=SHAPE_REPRESENTATION_RELATIONSHIP('SRR','None',#7542,#258);
#233=SHAPE_REPRESENTATION_RELATIONSHIP('SRR','None',#7543,#259);
#234=SHAPE_REPRESENTATION_RELATIONSHIP('SRR','None',#7544,#260);
#235=SHAPE_REPRESENTATION_RELATIONSHIP('SRR','None',#7545,#261);
#236=SHAPE_REPRESENTATION_RELATIONSHIP('SRR','None',#7546,#262);
#237=SHAPE_REPRESENTATION_RELATIONSHIP('SRR','None',#7547,#263);
#238=SHAPE_REPRESENTATION_RELATIONSHIP('SRR','None',#7548,#264);
#239=SHAPE_REPRESENTATION_RELATIONSHIP('SRR','None',#7549,#265);
#240=SHAPE_REPRESENTATION_RELATIONSHIP('SRR','None',#7550,#266);
#241=SHAPE_REPRESENTATION_RELATIONSHIP('SRR','None',#7551,#267);
#242=SHAPE_REPRESENTATION_RELATIONSHIP('SRR','None',#7552,#268);
#243=SHAPE_REPRESENTATION_RELATIONSHIP('SRR','None',#7553,#269);
#244=SHAPE_REPRESENTATION_RELATIONSHIP('SRR','None',#7554,#270);
#245=SHAPE_REPRESENTATION_RELATIONSHIP('SRR','None',#7556,#271);
#246=SHAPE_REPRESENTATION_RELATIONSHIP('SRR','None',#7557,#272);
#247=SHAPE_REPRESENTATION_RELATIONSHIP('SRR','None',#7558,#273);
#248=SHAPE_REPRESENTATION_RELATIONSHIP('SRR','None',#7559,#274);
#249=SHAPE_REPRESENTATION_RELATIONSHIP('SRR','None',#7560,#275);
#250=SHAPE_REPRESENTATION_RELATIONSHIP('SRR','None',#7561,#276);
#251=ADVANCED_BREP_SHAPE_REPRESENTATION('',(#303),#7398);
#252=ADVANCED_BREP_SHAPE_REPRESENTATION('',(#304),#7399);
#253=ADVANCED_BREP_SHAPE_REPRESENTATION('',(#305),#7400);
#254=ADVANCED_BREP_SHAPE_REPRESENTATION('',(#306),#7401);
#255=ADVANCED_BREP_SHAPE_REPRESENTATION('',(#307),#7402);
#256=ADVANCED_BREP_SHAPE_REPRESENTATION('',(#308),#7403);
#257=ADVANCED_BREP_SHAPE_REPRESENTATION('',(#309),#7404);
#258=ADVANCED_BREP_SHAPE_REPRESENTATION('',(#310),#7405);
#259=ADVANCED_BREP_SHAPE_REPRESENTATION('',(#311),#7406);
#260=ADVANCED_BREP_SHAPE_REPRESENTATION('',(#312),#7407);
#261=ADVANCED_BREP_SHAPE_REPRESENTATION('',(#313),#7408);
#262=ADVANCED_BREP_SHAPE_REPRESENTATION('',(#314),#7409);
#263=ADVANCED_BREP_SHAPE_REPRESENTATION('',(#315),#7410);
#264=ADVANCED_BREP_SHAPE_REPRESENTATION('',(#316),#7411);
#265=ADVANCED_BREP_SHAPE_REPRESENTATION('',(#317),#7412);
#266=ADVANCED_BREP_SHAPE_REPRESENTATION('',(#221),#7413);
#267=ADVANCED_BREP_SHAPE_REPRESENTATION('',(#318),#7414);
#268=ADVANCED_BREP_SHAPE_REPRESENTATION('',(#319),#7415);
#269=ADVANCED_BREP_SHAPE_REPRESENTATION('',(#320),#7416);
#270=ADVANCED_BREP_SHAPE_REPRESENTATION('',(#222),#7417);
#271=ADVANCED_BREP_SHAPE_REPRESENTATION('',(#321),#7419);
#272=ADVANCED_BREP_SHAPE_REPRESENTATION('',(#322),#7420);
#273=ADVANCED_BREP_SHAPE_REPRESENTATION('',(#323),#7421);
#274=ADVANCED_BREP_SHAPE_REPRESENTATION('',(#324),#7422);
#275=ADVANCED_BREP_SHAPE_REPRESENTATION('',(#325),#7423);
#276=ADVANCED_BREP_SHAPE_REPRESENTATION('',(#223),#7424);
#277=STYLED_ITEM('',(#7723),#303);
#278=STYLED_ITEM('',(#7730),#304);
#279=STYLED_ITEM('',(#7723),#305);
#280=STYLED_ITEM('',(#7730),#306);
#281=STYLED_ITEM('',(#7723),#307);
#282=STYLED_ITEM('',(#7737),#308);
#283=STYLED_ITEM('',(#7737),#309);
#284=STYLED_ITEM('',(#7730),#310);
#285=STYLED_ITEM('',(#7730),#311);
#286=STYLED_ITEM('',(#7737),#312);
#287=STYLED_ITEM('',(#7737),#313);
#288=STYLED_ITEM('',(#7737),#314);
#289=STYLED_ITEM('',(#7737),#315);
#290=STYLED_ITEM('',(#7744),#316);
#291=STYLED_ITEM('',(#7744),#317);
#292=STYLED_ITEM('',(#7751),#221);
#293=STYLED_ITEM('',(#7751),#318);
#294=STYLED_ITEM('',(#7751),#319);
#295=STYLED_ITEM('',(#7730),#320);
#296=STYLED_ITEM('',(#7751),#222);
#297=STYLED_ITEM('',(#7730),#321);
#298=STYLED_ITEM('',(#7737),#322);
#299=STYLED_ITEM('',(#7758),#323);
#300=STYLED_ITEM('',(#7737),#324);
#301=STYLED_ITEM('',(#7751),#325);
#302=STYLED_ITEM('',(#7751),#223);
#303=MANIFOLD_SOLID_BREP('Body1',#4082);
#304=MANIFOLD_SOLID_BREP('Body1',#4083);
#305=MANIFOLD_SOLID_BREP('Body1',#4084);
#306=MANIFOLD_SOLID_BREP('Body1',#4085);
#307=MANIFOLD_SOLID_BREP('Body1',#4086);
#308=MANIFOLD_SOLID_BREP('Body1',#4087);
#309=MANIFOLD_SOLID_BREP('Body1',#4088);
#310=MANIFOLD_SOLID_BREP('Body1',#4089);
#311=MANIFOLD_SOLID_BREP('Body1',#4090);
#312=MANIFOLD_SOLID_BREP('Body1',#4091);
#313=MANIFOLD_SOLID_BREP('Body1',#4092);
#314=MANIFOLD_SOLID_BREP('Body1',#4093);
#315=MANIFOLD_SOLID_BREP('Body1',#4094);
#316=MANIFOLD_SOLID_BREP('Body1',#4095);
#317=MANIFOLD_SOLID_BREP('Body1',#4096);
#318=MANIFOLD_SOLID_BREP('Body1',#4099);
#319=MANIFOLD_SOLID_BREP('Body1',#4100);
#320=MANIFOLD_SOLID_BREP('Body1',#4101);
#321=MANIFOLD_SOLID_BREP('Body1',#4104);
#322=MANIFOLD_SOLID_BREP('Body1',#4105);
#323=MANIFOLD_SOLID_BREP('Body1',#4106);
#324=MANIFOLD_SOLID_BREP('Body1',#4107);
#325=MANIFOLD_SOLID_BREP('Body1',#4108);
#326=SPHERICAL_SURFACE('',#4436,1.6);
#327=SPHERICAL_SURFACE('',#4444,1.5);
#328=SPHERICAL_SURFACE('',#4490,1.6);
#329=SPHERICAL_SURFACE('',#4498,1.5);
#330=SPHERICAL_SURFACE('',#4800,1.5);
#331=FACE_BOUND('',#839,.T.);
#332=FACE_BOUND('',#840,.T.);
#333=FACE_BOUND('',#844,.T.);
#334=FACE_BOUND('',#846,.T.);
#335=FACE_BOUND('',#848,.T.);
#336=FACE_BOUND('',#850,.T.);
#337=FACE_BOUND('',#851,.T.);
#338=FACE_BOUND('',#852,.T.);
#339=FACE_BOUND('',#853,.T.);
#340=FACE_BOUND('',#856,.T.);
#341=FACE_BOUND('',#857,.T.);
#342=FACE_BOUND('',#858,.T.);
#343=FACE_BOUND('',#859,.T.);
#344=FACE_BOUND('',#860,.T.);
#345=FACE_BOUND('',#864,.T.);
#346=FACE_BOUND('',#868,.T.);
#347=FACE_BOUND('',#870,.T.);
#348=FACE_BOUND('',#882,.T.);
#349=FACE_BOUND('',#883,.T.);
#350=FACE_BOUND('',#887,.T.);
#351=FACE_BOUND('',#889,.T.);
#352=FACE_BOUND('',#891,.T.);
#353=FACE_BOUND('',#893,.T.);
#354=FACE_BOUND('',#894,.T.);
#355=FACE_BOUND('',#895,.T.);
#356=FACE_BOUND('',#896,.T.);
#357=FACE_BOUND('',#897,.T.);
#358=FACE_BOUND('',#900,.T.);
#359=FACE_BOUND('',#901,.T.);
#360=FACE_BOUND('',#902,.T.);
#361=FACE_BOUND('',#903,.T.);
#362=FACE_BOUND('',#907,.T.);
#363=FACE_BOUND('',#911,.T.);
#364=FACE_BOUND('',#913,.T.);
#365=FACE_BOUND('',#923,.T.);
#366=FACE_BOUND('',#924,.T.);
#367=FACE_BOUND('',#925,.T.);
#368=FACE_BOUND('',#926,.T.);
#369=FACE_BOUND('',#934,.T.);
#370=FACE_BOUND('',#935,.T.);
#371=FACE_BOUND('',#936,.T.);
#372=FACE_BOUND('',#937,.T.);
#373=FACE_BOUND('',#939,.T.);
#374=FACE_BOUND('',#942,.T.);
#375=FACE_BOUND('',#946,.T.);
#376=FACE_BOUND('',#950,.T.);
#377=FACE_BOUND('',#954,.T.);
#378=FACE_BOUND('',#956,.T.);
#379=FACE_BOUND('',#971,.T.);
#380=FACE_BOUND('',#972,.T.);
#381=FACE_BOUND('',#973,.T.);
#382=FACE_BOUND('',#974,.T.);
#383=FACE_BOUND('',#975,.T.);
#384=FACE_BOUND('',#976,.T.);
#385=FACE_BOUND('',#977,.T.);
#386=FACE_BOUND('',#979,.T.);
#387=FACE_BOUND('',#980,.T.);
#388=FACE_BOUND('',#981,.T.);
#389=FACE_BOUND('',#982,.T.);
#390=FACE_BOUND('',#983,.T.);
#391=FACE_BOUND('',#987,.T.);
#392=FACE_BOUND('',#989,.T.);
#393=FACE_BOUND('',#993,.T.);
#394=FACE_BOUND('',#995,.T.);
#395=FACE_BOUND('',#999,.T.);
#396=FACE_BOUND('',#1001,.T.);
#397=FACE_BOUND('',#1005,.T.);
#398=FACE_BOUND('',#1007,.T.);
#399=FACE_BOUND('',#1023,.T.);
#400=FACE_BOUND('',#1031,.T.);
#401=FACE_BOUND('',#1037,.T.);
#402=FACE_BOUND('',#1040,.T.);
#403=FACE_BOUND('',#1051,.T.);
#404=FACE_BOUND('',#1053,.T.);
#405=FACE_BOUND('',#1055,.T.);
#406=FACE_BOUND('',#1057,.T.);
#407=FACE_BOUND('',#1066,.T.);
#408=FACE_BOUND('',#1071,.T.);
#409=FACE_BOUND('',#1078,.T.);
#410=FACE_BOUND('',#1098,.T.);
#411=FACE_BOUND('',#1099,.T.);
#412=FACE_BOUND('',#1111,.T.);
#413=FACE_BOUND('',#1123,.T.);
#414=FACE_BOUND('',#1133,.T.);
#415=FACE_BOUND('',#1135,.T.);
#416=FACE_BOUND('',#1139,.T.);
#417=FACE_BOUND('',#1141,.T.);
#418=FACE_BOUND('',#1162,.T.);
#419=PLANE('',#4404);
#420=PLANE('',#4408);
#421=PLANE('',#4424);
#422=PLANE('',#4426);
#423=PLANE('',#4433);
#424=PLANE('',#4435);
#425=PLANE('',#4438);
#426=PLANE('',#4439);
#427=PLANE('',#4440);
#428=PLANE('',#4441);
#429=PLANE('',#4442);
#430=PLANE('',#4452);
#431=PLANE('',#4453);
#432=PLANE('',#4458);
#433=PLANE('',#4462);
#434=PLANE('',#4478);
#435=PLANE('',#4480);
#436=PLANE('',#4487);
#437=PLANE('',#4488);
#438=PLANE('',#4492);
#439=PLANE('',#4493);
#440=PLANE('',#4494);
#441=PLANE('',#4495);
#442=PLANE('',#4496);
#443=PLANE('',#4506);
#444=PLANE('',#4507);
#445=PLANE('',#4521);
#446=PLANE('',#4522);
#447=PLANE('',#4523);
#448=PLANE('',#4524);
#449=PLANE('',#4525);
#450=PLANE('',#4527);
#451=PLANE('',#4528);
#452=PLANE('',#4531);
#453=PLANE('',#4532);
#454=PLANE('',#4533);
#455=PLANE('',#4534);
#456=PLANE('',#4536);
#457=PLANE('',#4541);
#458=PLANE('',#4547);
#459=PLANE('',#4556);
#460=PLANE('',#4563);
#461=PLANE('',#4564);
#462=PLANE('',#4569);
#463=PLANE('',#4573);
#464=PLANE('',#4589);
#465=PLANE('',#4590);
#466=PLANE('',#4591);
#467=PLANE('',#4592);
#468=PLANE('',#4593);
#469=PLANE('',#4594);
#470=PLANE('',#4602);
#471=PLANE('',#4603);
#472=PLANE('',#4611);
#473=PLANE('',#4612);
#474=PLANE('',#4620);
#475=PLANE('',#4621);
#476=PLANE('',#4629);
#477=PLANE('',#4630);
#478=PLANE('',#4635);
#479=PLANE('',#4636);
#480=PLANE('',#4641);
#481=PLANE('',#4642);
#482=PLANE('',#4644);
#483=PLANE('',#4645);
#484=PLANE('',#4646);
#485=PLANE('',#4647);
#486=PLANE('',#4648);
#487=PLANE('',#4649);
#488=PLANE('',#4650);
#489=PLANE('',#4651);
#490=PLANE('',#4652);
#491=PLANE('',#4657);
#492=PLANE('',#4658);
#493=PLANE('',#4666);
#494=PLANE('',#4677);
#495=PLANE('',#4681);
#496=PLANE('',#4687);
#497=PLANE('',#4688);
#498=PLANE('',#4689);
#499=PLANE('',#4693);
#500=PLANE('',#4694);
#501=PLANE('',#4695);
#502=PLANE('',#4696);
#503=PLANE('',#4697);
#504=PLANE('',#4699);
#505=PLANE('',#4701);
#506=PLANE('',#4703);
#507=PLANE('',#4704);
#508=PLANE('',#4705);
#509=PLANE('',#4706);
#510=PLANE('',#4707);
#511=PLANE('',#4708);
#512=PLANE('',#4711);
#513=PLANE('',#4719);
#514=PLANE('',#4723);
#515=PLANE('',#4731);
#516=PLANE('',#4739);
#517=PLANE('',#4740);
#518=PLANE('',#4741);
#519=PLANE('',#4742);
#520=PLANE('',#4743);
#521=PLANE('',#4744);
#522=PLANE('',#4745);
#523=PLANE('',#4746);
#524=PLANE('',#4747);
#525=PLANE('',#4787);
#526=PLANE('',#4789);
#527=PLANE('',#4792);
#528=PLANE('',#4794);
#529=PLANE('',#4796);
#530=PLANE('',#4806);
#531=PLANE('',#4807);
#532=PLANE('',#4809);
#533=PLANE('',#4811);
#534=PLANE('',#4813);
#535=PLANE('',#4815);
#536=PLANE('',#4816);
#537=PLANE('',#4817);
#538=PLANE('',#4818);
#539=PLANE('',#4819);
#540=PLANE('',#4820);
#541=PLANE('',#4822);
#542=PLANE('',#4825);
#543=PLANE('',#4827);
#544=PLANE('',#4829);
#545=PLANE('',#4830);
#546=PLANE('',#4831);
#547=PLANE('',#4832);
#548=PLANE('',#4833);
#549=PLANE('',#4836);
#550=PLANE('',#4838);
#551=PLANE('',#4839);
#552=PLANE('',#4840);
#553=PLANE('',#4841);
#554=PLANE('',#4842);
#555=PLANE('',#4843);
#556=PLANE('',#4844);
#557=PLANE('',#4845);
#558=PLANE('',#4846);
#559=PLANE('',#4847);
#560=PLANE('',#4855);
#561=PLANE('',#4856);
#562=PLANE('',#4858);
#563=PLANE('',#4859);
#564=PLANE('',#4860);
#565=PLANE('',#4861);
#566=PLANE('',#4862);
#567=PLANE('',#4863);
#568=PLANE('',#4865);
#569=PLANE('',#4866);
#570=PLANE('',#4867);
#571=PLANE('',#4868);
#572=PLANE('',#4869);
#573=PLANE('',#4870);
#574=PLANE('',#4871);
#575=PLANE('',#4872);
#576=PLANE('',#4873);
#577=PLANE('',#4875);
#578=PLANE('',#4883);
#579=FACE_OUTER_BOUND('',#828,.T.);
#580=FACE_OUTER_BOUND('',#829,.T.);
#581=FACE_OUTER_BOUND('',#830,.T.);
#582=FACE_OUTER_BOUND('',#831,.T.);
#583=FACE_OUTER_BOUND('',#832,.T.);
#584=FACE_OUTER_BOUND('',#833,.T.);
#585=FACE_OUTER_BOUND('',#834,.T.);
#586=FACE_OUTER_BOUND('',#835,.T.);
#587=FACE_OUTER_BOUND('',#836,.T.);
#588=FACE_OUTER_BOUND('',#837,.T.);
#589=FACE_OUTER_BOUND('',#838,.T.);
#590=FACE_OUTER_BOUND('',#841,.T.);
#591=FACE_OUTER_BOUND('',#842,.T.);
#592=FACE_OUTER_BOUND('',#843,.T.);
#593=FACE_OUTER_BOUND('',#845,.T.);
#594=FACE_OUTER_BOUND('',#847,.T.);
#595=FACE_OUTER_BOUND('',#849,.T.);
#596=FACE_OUTER_BOUND('',#854,.T.);
#597=FACE_OUTER_BOUND('',#855,.T.);
#598=FACE_OUTER_BOUND('',#861,.T.);
#599=FACE_OUTER_BOUND('',#862,.T.);
#600=FACE_OUTER_BOUND('',#863,.T.);
#601=FACE_OUTER_BOUND('',#865,.T.);
#602=FACE_OUTER_BOUND('',#866,.T.);
#603=FACE_OUTER_BOUND('',#867,.T.);
#604=FACE_OUTER_BOUND('',#869,.T.);
#605=FACE_OUTER_BOUND('',#871,.T.);
#606=FACE_OUTER_BOUND('',#872,.T.);
#607=FACE_OUTER_BOUND('',#873,.T.);
#608=FACE_OUTER_BOUND('',#874,.T.);
#609=FACE_OUTER_BOUND('',#875,.T.);
#610=FACE_OUTER_BOUND('',#876,.T.);
#611=FACE_OUTER_BOUND('',#877,.T.);
#612=FACE_OUTER_BOUND('',#878,.T.);
#613=FACE_OUTER_BOUND('',#879,.T.);
#614=FACE_OUTER_BOUND('',#880,.T.);
#615=FACE_OUTER_BOUND('',#881,.T.);
#616=FACE_OUTER_BOUND('',#884,.T.);
#617=FACE_OUTER_BOUND('',#885,.T.);
#618=FACE_OUTER_BOUND('',#886,.T.);
#619=FACE_OUTER_BOUND('',#888,.T.);
#620=FACE_OUTER_BOUND('',#890,.T.);
#621=FACE_OUTER_BOUND('',#892,.T.);
#622=FACE_OUTER_BOUND('',#898,.T.);
#623=FACE_OUTER_BOUND('',#899,.T.);
#624=FACE_OUTER_BOUND('',#904,.T.);
#625=FACE_OUTER_BOUND('',#905,.T.);
#626=FACE_OUTER_BOUND('',#906,.T.);
#627=FACE_OUTER_BOUND('',#908,.T.);
#628=FACE_OUTER_BOUND('',#909,.T.);
#629=FACE_OUTER_BOUND('',#910,.T.);
#630=FACE_OUTER_BOUND('',#912,.T.);
#631=FACE_OUTER_BOUND('',#914,.T.);
#632=FACE_OUTER_BOUND('',#915,.T.);
#633=FACE_OUTER_BOUND('',#916,.T.);
#634=FACE_OUTER_BOUND('',#917,.T.);
#635=FACE_OUTER_BOUND('',#918,.T.);
#636=FACE_OUTER_BOUND('',#919,.T.);
#637=FACE_OUTER_BOUND('',#920,.T.);
#638=FACE_OUTER_BOUND('',#921,.T.);
#639=FACE_OUTER_BOUND('',#922,.T.);
#640=FACE_OUTER_BOUND('',#927,.T.);
#641=FACE_OUTER_BOUND('',#928,.T.);
#642=FACE_OUTER_BOUND('',#929,.T.);
#643=FACE_OUTER_BOUND('',#930,.T.);
#644=FACE_OUTER_BOUND('',#931,.T.);
#645=FACE_OUTER_BOUND('',#932,.T.);
#646=FACE_OUTER_BOUND('',#933,.T.);
#647=FACE_OUTER_BOUND('',#938,.T.);
#648=FACE_OUTER_BOUND('',#940,.T.);
#649=FACE_OUTER_BOUND('',#941,.T.);
#650=FACE_OUTER_BOUND('',#943,.T.);
#651=FACE_OUTER_BOUND('',#944,.T.);
#652=FACE_OUTER_BOUND('',#945,.T.);
#653=FACE_OUTER_BOUND('',#947,.T.);
#654=FACE_OUTER_BOUND('',#948,.T.);
#655=FACE_OUTER_BOUND('',#949,.T.);
#656=FACE_OUTER_BOUND('',#951,.T.);
#657=FACE_OUTER_BOUND('',#952,.T.);
#658=FACE_OUTER_BOUND('',#953,.T.);
#659=FACE_OUTER_BOUND('',#955,.T.);
#660=FACE_OUTER_BOUND('',#957,.T.);
#661=FACE_OUTER_BOUND('',#958,.T.);
#662=FACE_OUTER_BOUND('',#959,.T.);
#663=FACE_OUTER_BOUND('',#960,.T.);
#664=FACE_OUTER_BOUND('',#961,.T.);
#665=FACE_OUTER_BOUND('',#962,.T.);
#666=FACE_OUTER_BOUND('',#963,.T.);
#667=FACE_OUTER_BOUND('',#964,.T.);
#668=FACE_OUTER_BOUND('',#965,.T.);
#669=FACE_OUTER_BOUND('',#966,.T.);
#670=FACE_OUTER_BOUND('',#967,.T.);
#671=FACE_OUTER_BOUND('',#968,.T.);
#672=FACE_OUTER_BOUND('',#969,.T.);
#673=FACE_OUTER_BOUND('',#970,.T.);
#674=FACE_OUTER_BOUND('',#978,.T.);
#675=FACE_OUTER_BOUND('',#984,.T.);
#676=FACE_OUTER_BOUND('',#985,.T.);
#677=FACE_OUTER_BOUND('',#986,.T.);
#678=FACE_OUTER_BOUND('',#988,.T.);
#679=FACE_OUTER_BOUND('',#990,.T.);
#680=FACE_OUTER_BOUND('',#991,.T.);
#681=FACE_OUTER_BOUND('',#992,.T.);
#682=FACE_OUTER_BOUND('',#994,.T.);
#683=FACE_OUTER_BOUND('',#996,.T.);
#684=FACE_OUTER_BOUND('',#997,.T.);
#685=FACE_OUTER_BOUND('',#998,.T.);
#686=FACE_OUTER_BOUND('',#1000,.T.);
#687=FACE_OUTER_BOUND('',#1002,.T.);
#688=FACE_OUTER_BOUND('',#1003,.T.);
#689=FACE_OUTER_BOUND('',#1004,.T.);
#690=FACE_OUTER_BOUND('',#1006,.T.);
#691=FACE_OUTER_BOUND('',#1008,.T.);
#692=FACE_OUTER_BOUND('',#1009,.T.);
#693=FACE_OUTER_BOUND('',#1010,.T.);
#694=FACE_OUTER_BOUND('',#1011,.T.);
#695=FACE_OUTER_BOUND('',#1012,.T.);
#696=FACE_OUTER_BOUND('',#1013,.T.);
#697=FACE_OUTER_BOUND('',#1014,.T.);
#698=FACE_OUTER_BOUND('',#1015,.T.);
#699=FACE_OUTER_BOUND('',#1016,.T.);
#700=FACE_OUTER_BOUND('',#1017,.T.);
#701=FACE_OUTER_BOUND('',#1018,.T.);
#702=FACE_OUTER_BOUND('',#1019,.T.);
#703=FACE_OUTER_BOUND('',#1020,.T.);
#704=FACE_OUTER_BOUND('',#1021,.T.);
#705=FACE_OUTER_BOUND('',#1022,.T.);
#706=FACE_OUTER_BOUND('',#1024,.T.);
#707=FACE_OUTER_BOUND('',#1025,.T.);
#708=FACE_OUTER_BOUND('',#1026,.T.);
#709=FACE_OUTER_BOUND('',#1027,.T.);
#710=FACE_OUTER_BOUND('',#1028,.T.);
#711=FACE_OUTER_BOUND('',#1029,.T.);
#712=FACE_OUTER_BOUND('',#1030,.T.);
#713=FACE_OUTER_BOUND('',#1032,.T.);
#714=FACE_OUTER_BOUND('',#1033,.T.);
#715=FACE_OUTER_BOUND('',#1034,.T.);
#716=FACE_OUTER_BOUND('',#1035,.T.);
#717=FACE_OUTER_BOUND('',#1036,.T.);
#718=FACE_OUTER_BOUND('',#1038,.T.);
#719=FACE_OUTER_BOUND('',#1039,.T.);
#720=FACE_OUTER_BOUND('',#1041,.T.);
#721=FACE_OUTER_BOUND('',#1042,.T.);
#722=FACE_OUTER_BOUND('',#1043,.T.);
#723=FACE_OUTER_BOUND('',#1044,.T.);
#724=FACE_OUTER_BOUND('',#1045,.T.);
#725=FACE_OUTER_BOUND('',#1046,.T.);
#726=FACE_OUTER_BOUND('',#1047,.T.);
#727=FACE_OUTER_BOUND('',#1048,.T.);
#728=FACE_OUTER_BOUND('',#1049,.T.);
#729=FACE_OUTER_BOUND('',#1050,.T.);
#730=FACE_OUTER_BOUND('',#1052,.T.);
#731=FACE_OUTER_BOUND('',#1054,.T.);
#732=FACE_OUTER_BOUND('',#1056,.T.);
#733=FACE_OUTER_BOUND('',#1058,.T.);
#734=FACE_OUTER_BOUND('',#1059,.T.);
#735=FACE_OUTER_BOUND('',#1060,.T.);
#736=FACE_OUTER_BOUND('',#1061,.T.);
#737=FACE_OUTER_BOUND('',#1062,.T.);
#738=FACE_OUTER_BOUND('',#1063,.T.);
#739=FACE_OUTER_BOUND('',#1064,.T.);
#740=FACE_OUTER_BOUND('',#1065,.T.);
#741=FACE_OUTER_BOUND('',#1067,.T.);
#742=FACE_OUTER_BOUND('',#1068,.T.);
#743=FACE_OUTER_BOUND('',#1069,.T.);
#744=FACE_OUTER_BOUND('',#1070,.T.);
#745=FACE_OUTER_BOUND('',#1072,.T.);
#746=FACE_OUTER_BOUND('',#1073,.T.);
#747=FACE_OUTER_BOUND('',#1074,.T.);
#748=FACE_OUTER_BOUND('',#1075,.T.);
#749=FACE_OUTER_BOUND('',#1076,.T.);
#750=FACE_OUTER_BOUND('',#1077,.T.);
#751=FACE_OUTER_BOUND('',#1079,.T.);
#752=FACE_OUTER_BOUND('',#1080,.T.);
#753=FACE_OUTER_BOUND('',#1081,.T.);
#754=FACE_OUTER_BOUND('',#1082,.T.);
#755=FACE_OUTER_BOUND('',#1083,.T.);
#756=FACE_OUTER_BOUND('',#1084,.T.);
#757=FACE_OUTER_BOUND('',#1085,.T.);
#758=FACE_OUTER_BOUND('',#1086,.T.);
#759=FACE_OUTER_BOUND('',#1087,.T.);
#760=FACE_OUTER_BOUND('',#1088,.T.);
#761=FACE_OUTER_BOUND('',#1089,.T.);
#762=FACE_OUTER_BOUND('',#1090,.T.);
#763=FACE_OUTER_BOUND('',#1091,.T.);
#764=FACE_OUTER_BOUND('',#1092,.T.);
#765=FACE_OUTER_BOUND('',#1093,.T.);
#766=FACE_OUTER_BOUND('',#1094,.T.);
#767=FACE_OUTER_BOUND('',#1095,.T.);
#768=FACE_OUTER_BOUND('',#1096,.T.);
#769=FACE_OUTER_BOUND('',#1097,.T.);
#770=FACE_OUTER_BOUND('',#1100,.T.);
#771=FACE_OUTER_BOUND('',#1101,.T.);
#772=FACE_OUTER_BOUND('',#1102,.T.);
#773=FACE_OUTER_BOUND('',#1103,.T.);
#774=FACE_OUTER_BOUND('',#1104,.T.);
#775=FACE_OUTER_BOUND('',#1105,.T.);
#776=FACE_OUTER_BOUND('',#1106,.T.);
#777=FACE_OUTER_BOUND('',#1107,.T.);
#778=FACE_OUTER_BOUND('',#1108,.T.);
#779=FACE_OUTER_BOUND('',#1109,.T.);
#780=FACE_OUTER_BOUND('',#1110,.T.);
#781=FACE_OUTER_BOUND('',#1112,.T.);
#782=FACE_OUTER_BOUND('',#1113,.T.);
#783=FACE_OUTER_BOUND('',#1114,.T.);
#784=FACE_OUTER_BOUND('',#1115,.T.);
#785=FACE_OUTER_BOUND('',#1116,.T.);
#786=FACE_OUTER_BOUND('',#1117,.T.);
#787=FACE_OUTER_BOUND('',#1118,.T.);
#788=FACE_OUTER_BOUND('',#1119,.T.);
#789=FACE_OUTER_BOUND('',#1120,.T.);
#790=FACE_OUTER_BOUND('',#1121,.T.);
#791=FACE_OUTER_BOUND('',#1122,.T.);
#792=FACE_OUTER_BOUND('',#1124,.T.);
#793=FACE_OUTER_BOUND('',#1125,.T.);
#794=FACE_OUTER_BOUND('',#1126,.T.);
#795=FACE_OUTER_BOUND('',#1127,.T.);
#796=FACE_OUTER_BOUND('',#1128,.T.);
#797=FACE_OUTER_BOUND('',#1129,.T.);
#798=FACE_OUTER_BOUND('',#1130,.T.);
#799=FACE_OUTER_BOUND('',#1131,.T.);
#800=FACE_OUTER_BOUND('',#1132,.T.);
#801=FACE_OUTER_BOUND('',#1134,.T.);
#802=FACE_OUTER_BOUND('',#1136,.T.);
#803=FACE_OUTER_BOUND('',#1137,.T.);
#804=FACE_OUTER_BOUND('',#1138,.T.);
#805=FACE_OUTER_BOUND('',#1140,.T.);
#806=FACE_OUTER_BOUND('',#1142,.T.);
#807=FACE_OUTER_BOUND('',#1143,.T.);
#808=FACE_OUTER_BOUND('',#1144,.T.);
#809=FACE_OUTER_BOUND('',#1145,.T.);
#810=FACE_OUTER_BOUND('',#1146,.T.);
#811=FACE_OUTER_BOUND('',#1147,.T.);
#812=FACE_OUTER_BOUND('',#1148,.T.);
#813=FACE_OUTER_BOUND('',#1149,.T.);
#814=FACE_OUTER_BOUND('',#1150,.T.);
#815=FACE_OUTER_BOUND('',#1151,.T.);
#816=FACE_OUTER_BOUND('',#1152,.T.);
#817=FACE_OUTER_BOUND('',#1153,.T.);
#818=FACE_OUTER_BOUND('',#1154,.T.);
#819=FACE_OUTER_BOUND('',#1155,.T.);
#820=FACE_OUTER_BOUND('',#1156,.T.);
#821=FACE_OUTER_BOUND('',#1157,.T.);
#822=FACE_OUTER_BOUND('',#1158,.T.);
#823=FACE_OUTER_BOUND('',#1159,.T.);
#824=FACE_OUTER_BOUND('',#1160,.T.);
#825=FACE_OUTER_BOUND('',#1161,.T.);
#826=FACE_OUTER_BOUND('',#1163,.T.);
#827=FACE_OUTER_BOUND('',#1164,.T.);
#828=EDGE_LOOP('',(#2775,#2776,#2777,#2778));
#829=EDGE_LOOP('',(#2779));
#830=EDGE_LOOP('',(#2780,#2781,#2782,#2783));
#831=EDGE_LOOP('',(#2784));
#832=EDGE_LOOP('',(#2785,#2786,#2787,#2788));
#833=EDGE_LOOP('',(#2789,#2790,#2791,#2792));
#834=EDGE_LOOP('',(#2793,#2794,#2795,#2796));
#835=EDGE_LOOP('',(#2797,#2798,#2799,#2800));
#836=EDGE_LOOP('',(#2801,#2802,#2803,#2804));
#837=EDGE_LOOP('',(#2805,#2806,#2807,#2808));
#838=EDGE_LOOP('',(#2809,#2810,#2811,#2812,#2813,#2814));
#839=EDGE_LOOP('',(#2815));
#840=EDGE_LOOP('',(#2816));
#841=EDGE_LOOP('',(#2817,#2818,#2819,#2820));
#842=EDGE_LOOP('',(#2821,#2822,#2823,#2824));
#843=EDGE_LOOP('',(#2825));
#844=EDGE_LOOP('',(#2826));
#845=EDGE_LOOP('',(#2827));
#846=EDGE_LOOP('',(#2828));
#847=EDGE_LOOP('',(#2829,#2830));
#848=EDGE_LOOP('',(#2831));
#849=EDGE_LOOP('',(#2832,#2833,#2834,#2835,#2836,#2837,#2838,#2839,#2840,
#2841));
#850=EDGE_LOOP('',(#2842));
#851=EDGE_LOOP('',(#2843));
#852=EDGE_LOOP('',(#2844));
#853=EDGE_LOOP('',(#2845));
#854=EDGE_LOOP('',(#2846,#2847,#2848,#2849));
#855=EDGE_LOOP('',(#2850,#2851,#2852,#2853));
#856=EDGE_LOOP('',(#2854));
#857=EDGE_LOOP('',(#2855));
#858=EDGE_LOOP('',(#2856));
#859=EDGE_LOOP('',(#2857));
#860=EDGE_LOOP('',(#2858));
#861=EDGE_LOOP('',(#2859,#2860,#2861,#2862));
#862=EDGE_LOOP('',(#2863,#2864,#2865,#2866));
#863=EDGE_LOOP('',(#2867));
#864=EDGE_LOOP('',(#2868));
#865=EDGE_LOOP('',(#2869,#2870,#2871,#2872));
#866=EDGE_LOOP('',(#2873,#2874,#2875,#2876));
#867=EDGE_LOOP('',(#2877));
#868=EDGE_LOOP('',(#2878));
#869=EDGE_LOOP('',(#2879));
#870=EDGE_LOOP('',(#2880));
#871=EDGE_LOOP('',(#2881,#2882,#2883,#2884));
#872=EDGE_LOOP('',(#2885));
#873=EDGE_LOOP('',(#2886,#2887,#2888,#2889));
#874=EDGE_LOOP('',(#2890));
#875=EDGE_LOOP('',(#2891,#2892,#2893,#2894));
#876=EDGE_LOOP('',(#2895,#2896,#2897,#2898));
#877=EDGE_LOOP('',(#2899,#2900,#2901,#2902));
#878=EDGE_LOOP('',(#2903,#2904,#2905,#2906));
#879=EDGE_LOOP('',(#2907,#2908,#2909,#2910));
#880=EDGE_LOOP('',(#2911,#2912,#2913,#2914));
#881=EDGE_LOOP('',(#2915,#2916,#2917,#2918,#2919,#2920));
#882=EDGE_LOOP('',(#2921));
#883=EDGE_LOOP('',(#2922));
#884=EDGE_LOOP('',(#2923,#2924,#2925,#2926));
#885=EDGE_LOOP('',(#2927,#2928,#2929,#2930));
#886=EDGE_LOOP('',(#2931));
#887=EDGE_LOOP('',(#2932));
#888=EDGE_LOOP('',(#2933));
#889=EDGE_LOOP('',(#2934));
#890=EDGE_LOOP('',(#2935,#2936));
#891=EDGE_LOOP('',(#2937));
#892=EDGE_LOOP('',(#2938,#2939,#2940,#2941));
#893=EDGE_LOOP('',(#2942));
#894=EDGE_LOOP('',(#2943));
#895=EDGE_LOOP('',(#2944));
#896=EDGE_LOOP('',(#2945));
#897=EDGE_LOOP('',(#2946));
#898=EDGE_LOOP('',(#2947,#2948,#2949,#2950));
#899=EDGE_LOOP('',(#2951,#2952,#2953,#2954,#2955,#2956,#2957,#2958,#2959,
#2960));
#900=EDGE_LOOP('',(#2961));
#901=EDGE_LOOP('',(#2962));
#902=EDGE_LOOP('',(#2963));
#903=EDGE_LOOP('',(#2964));
#904=EDGE_LOOP('',(#2965,#2966,#2967,#2968));
#905=EDGE_LOOP('',(#2969,#2970,#2971,#2972));
#906=EDGE_LOOP('',(#2973));
#907=EDGE_LOOP('',(#2974));
#908=EDGE_LOOP('',(#2975,#2976,#2977,#2978));
#909=EDGE_LOOP('',(#2979,#2980,#2981,#2982));
#910=EDGE_LOOP('',(#2983));
#911=EDGE_LOOP('',(#2984));
#912=EDGE_LOOP('',(#2985));
#913=EDGE_LOOP('',(#2986));
#914=EDGE_LOOP('',(#2987,#2988,#2989,#2990));
#915=EDGE_LOOP('',(#2991,#2992,#2993,#2994));
#916=EDGE_LOOP('',(#2995,#2996,#2997,#2998));
#917=EDGE_LOOP('',(#2999,#3000,#3001,#3002));
#918=EDGE_LOOP('',(#3003,#3004,#3005,#3006));
#919=EDGE_LOOP('',(#3007,#3008,#3009,#3010));
#920=EDGE_LOOP('',(#3011,#3012,#3013,#3014));
#921=EDGE_LOOP('',(#3015,#3016,#3017,#3018));
#922=EDGE_LOOP('',(#3019,#3020,#3021,#3022,#3023,#3024,#3025,#3026,#3027,
#3028));
#923=EDGE_LOOP('',(#3029));
#924=EDGE_LOOP('',(#3030));
#925=EDGE_LOOP('',(#3031));
#926=EDGE_LOOP('',(#3032));
#927=EDGE_LOOP('',(#3033,#3034,#3035,#3036));
#928=EDGE_LOOP('',(#3037,#3038,#3039,#3040));
#929=EDGE_LOOP('',(#3041,#3042,#3043,#3044));
#930=EDGE_LOOP('',(#3045,#3046,#3047,#3048));
#931=EDGE_LOOP('',(#3049,#3050,#3051,#3052));
#932=EDGE_LOOP('',(#3053,#3054,#3055,#3056));
#933=EDGE_LOOP('',(#3057,#3058,#3059,#3060,#3061,#3062,#3063,#3064,#3065,
#3066));
#934=EDGE_LOOP('',(#3067));
#935=EDGE_LOOP('',(#3068));
#936=EDGE_LOOP('',(#3069));
#937=EDGE_LOOP('',(#3070));
#938=EDGE_LOOP('',(#3071));
#939=EDGE_LOOP('',(#3072));
#940=EDGE_LOOP('',(#3073,#3074,#3075,#3076));
#941=EDGE_LOOP('',(#3077));
#942=EDGE_LOOP('',(#3078));
#943=EDGE_LOOP('',(#3079,#3080,#3081,#3082));
#944=EDGE_LOOP('',(#3083,#3084,#3085,#3086));
#945=EDGE_LOOP('',(#3087));
#946=EDGE_LOOP('',(#3088));
#947=EDGE_LOOP('',(#3089,#3090,#3091,#3092));
#948=EDGE_LOOP('',(#3093,#3094,#3095,#3096));
#949=EDGE_LOOP('',(#3097));
#950=EDGE_LOOP('',(#3098));
#951=EDGE_LOOP('',(#3099,#3100,#3101,#3102));
#952=EDGE_LOOP('',(#3103,#3104,#3105,#3106));
#953=EDGE_LOOP('',(#3107));
#954=EDGE_LOOP('',(#3108));
#955=EDGE_LOOP('',(#3109));
#956=EDGE_LOOP('',(#3110));
#957=EDGE_LOOP('',(#3111,#3112,#3113,#3114));
#958=EDGE_LOOP('',(#3115));
#959=EDGE_LOOP('',(#3116,#3117,#3118,#3119));
#960=EDGE_LOOP('',(#3120));
#961=EDGE_LOOP('',(#3121,#3122,#3123,#3124));
#962=EDGE_LOOP('',(#3125,#3126,#3127,#3128));
#963=EDGE_LOOP('',(#3129,#3130,#3131,#3132));
#964=EDGE_LOOP('',(#3133,#3134,#3135,#3136));
#965=EDGE_LOOP('',(#3137,#3138,#3139,#3140));
#966=EDGE_LOOP('',(#3141,#3142,#3143,#3144));
#967=EDGE_LOOP('',(#3145,#3146,#3147,#3148));
#968=EDGE_LOOP('',(#3149,#3150,#3151,#3152));
#969=EDGE_LOOP('',(#3153,#3154,#3155,#3156));
#970=EDGE_LOOP('',(#3157,#3158,#3159,#3160));
#971=EDGE_LOOP('',(#3161));
#972=EDGE_LOOP('',(#3162));
#973=EDGE_LOOP('',(#3163));
#974=EDGE_LOOP('',(#3164));
#975=EDGE_LOOP('',(#3165));
#976=EDGE_LOOP('',(#3166));
#977=EDGE_LOOP('',(#3167));
#978=EDGE_LOOP('',(#3168,#3169,#3170,#3171));
#979=EDGE_LOOP('',(#3172));
#980=EDGE_LOOP('',(#3173));
#981=EDGE_LOOP('',(#3174));
#982=EDGE_LOOP('',(#3175));
#983=EDGE_LOOP('',(#3176));
#984=EDGE_LOOP('',(#3177,#3178,#3179,#3180));
#985=EDGE_LOOP('',(#3181,#3182,#3183,#3184));
#986=EDGE_LOOP('',(#3185));
#987=EDGE_LOOP('',(#3186));
#988=EDGE_LOOP('',(#3187));
#989=EDGE_LOOP('',(#3188));
#990=EDGE_LOOP('',(#3189,#3190,#3191,#3192));
#991=EDGE_LOOP('',(#3193,#3194,#3195,#3196));
#992=EDGE_LOOP('',(#3197));
#993=EDGE_LOOP('',(#3198));
#994=EDGE_LOOP('',(#3199));
#995=EDGE_LOOP('',(#3200));
#996=EDGE_LOOP('',(#3201,#3202,#3203,#3204));
#997=EDGE_LOOP('',(#3205,#3206,#3207,#3208));
#998=EDGE_LOOP('',(#3209));
#999=EDGE_LOOP('',(#3210));
#1000=EDGE_LOOP('',(#3211));
#1001=EDGE_LOOP('',(#3212));
#1002=EDGE_LOOP('',(#3213,#3214,#3215,#3216));
#1003=EDGE_LOOP('',(#3217,#3218,#3219,#3220));
#1004=EDGE_LOOP('',(#3221));
#1005=EDGE_LOOP('',(#3222));
#1006=EDGE_LOOP('',(#3223));
#1007=EDGE_LOOP('',(#3224));
#1008=EDGE_LOOP('',(#3225,#3226,#3227,#3228));
#1009=EDGE_LOOP('',(#3229));
#1010=EDGE_LOOP('',(#3230));
#1011=EDGE_LOOP('',(#3231,#3232,#3233,#3234));
#1012=EDGE_LOOP('',(#3235));
#1013=EDGE_LOOP('',(#3236));
#1014=EDGE_LOOP('',(#3237,#3238,#3239,#3240));
#1015=EDGE_LOOP('',(#3241,#3242,#3243,#3244));
#1016=EDGE_LOOP('',(#3245,#3246,#3247,#3248));
#1017=EDGE_LOOP('',(#3249,#3250,#3251,#3252));
#1018=EDGE_LOOP('',(#3253,#3254,#3255,#3256));
#1019=EDGE_LOOP('',(#3257,#3258,#3259,#3260));
#1020=EDGE_LOOP('',(#3261,#3262,#3263,#3264,#3265,#3266));
#1021=EDGE_LOOP('',(#3267,#3268,#3269,#3270,#3271,#3272));
#1022=EDGE_LOOP('',(#3273));
#1023=EDGE_LOOP('',(#3274));
#1024=EDGE_LOOP('',(#3275,#3276,#3277,#3278));
#1025=EDGE_LOOP('',(#3279));
#1026=EDGE_LOOP('',(#3280));
#1027=EDGE_LOOP('',(#3281,#3282,#3283,#3284));
#1028=EDGE_LOOP('',(#3285,#3286,#3287,#3288));
#1029=EDGE_LOOP('',(#3289,#3290,#3291,#3292));
#1030=EDGE_LOOP('',(#3293));
#1031=EDGE_LOOP('',(#3294));
#1032=EDGE_LOOP('',(#3295,#3296,#3297,#3298));
#1033=EDGE_LOOP('',(#3299,#3300,#3301,#3302));
#1034=EDGE_LOOP('',(#3303,#3304,#3305,#3306));
#1035=EDGE_LOOP('',(#3307,#3308,#3309,#3310));
#1036=EDGE_LOOP('',(#3311));
#1037=EDGE_LOOP('',(#3312));
#1038=EDGE_LOOP('',(#3313,#3314,#3315,#3316));
#1039=EDGE_LOOP('',(#3317));
#1040=EDGE_LOOP('',(#3318));
#1041=EDGE_LOOP('',(#3319,#3320,#3321,#3322,#3323,#3324,#3325,#3326,#3327));
#1042=EDGE_LOOP('',(#3328,#3329,#3330,#3331,#3332,#3333,#3334,#3335,#3336));
#1043=EDGE_LOOP('',(#3337,#3338,#3339,#3340));
#1044=EDGE_LOOP('',(#3341,#3342,#3343,#3344));
#1045=EDGE_LOOP('',(#3345,#3346,#3347,#3348));
#1046=EDGE_LOOP('',(#3349,#3350,#3351,#3352));
#1047=EDGE_LOOP('',(#3353,#3354,#3355,#3356));
#1048=EDGE_LOOP('',(#3357,#3358,#3359,#3360));
#1049=EDGE_LOOP('',(#3361,#3362,#3363,#3364));
#1050=EDGE_LOOP('',(#3365));
#1051=EDGE_LOOP('',(#3366));
#1052=EDGE_LOOP('',(#3367));
#1053=EDGE_LOOP('',(#3368));
#1054=EDGE_LOOP('',(#3369,#3370,#3371,#3372,#3373,#3374));
#1055=EDGE_LOOP('',(#3375));
#1056=EDGE_LOOP('',(#3376,#3377,#3378,#3379,#3380,#3381));
#1057=EDGE_LOOP('',(#3382));
#1058=EDGE_LOOP('',(#3383,#3384,#3385,#3386));
#1059=EDGE_LOOP('',(#3387,#3388,#3389,#3390));
#1060=EDGE_LOOP('',(#3391,#3392,#3393,#3394));
#1061=EDGE_LOOP('',(#3395,#3396,#3397,#3398));
#1062=EDGE_LOOP('',(#3399,#3400,#3401,#3402));
#1063=EDGE_LOOP('',(#3403,#3404,#3405,#3406));
#1064=EDGE_LOOP('',(#3407,#3408,#3409,#3410));
#1065=EDGE_LOOP('',(#3411));
#1066=EDGE_LOOP('',(#3412));
#1067=EDGE_LOOP('',(#3413,#3414,#3415,#3416));
#1068=EDGE_LOOP('',(#3417,#3418,#3419,#3420));
#1069=EDGE_LOOP('',(#3421,#3422,#3423,#3424));
#1070=EDGE_LOOP('',(#3425));
#1071=EDGE_LOOP('',(#3426));
#1072=EDGE_LOOP('',(#3427,#3428,#3429,#3430));
#1073=EDGE_LOOP('',(#3431));
#1074=EDGE_LOOP('',(#3432,#3433,#3434,#3435));
#1075=EDGE_LOOP('',(#3436,#3437,#3438,#3439));
#1076=EDGE_LOOP('',(#3440,#3441,#3442,#3443));
#1077=EDGE_LOOP('',(#3444));
#1078=EDGE_LOOP('',(#3445));
#1079=EDGE_LOOP('',(#3446,#3447,#3448,#3449));
#1080=EDGE_LOOP('',(#3450,#3451,#3452,#3453));
#1081=EDGE_LOOP('',(#3454,#3455,#3456,#3457));
#1082=EDGE_LOOP('',(#3458));
#1083=EDGE_LOOP('',(#3459,#3460,#3461,#3462));
#1084=EDGE_LOOP('',(#3463,#3464,#3465,#3466));
#1085=EDGE_LOOP('',(#3467,#3468,#3469,#3470));
#1086=EDGE_LOOP('',(#3471,#3472,#3473,#3474));
#1087=EDGE_LOOP('',(#3475,#3476,#3477,#3478));
#1088=EDGE_LOOP('',(#3479,#3480,#3481,#3482));
#1089=EDGE_LOOP('',(#3483,#3484,#3485,#3486,#3487,#3488));
#1090=EDGE_LOOP('',(#3489,#3490,#3491,#3492,#3493,#3494));
#1091=EDGE_LOOP('',(#3495,#3496,#3497,#3498));
#1092=EDGE_LOOP('',(#3499,#3500,#3501,#3502,#3503));
#1093=EDGE_LOOP('',(#3504,#3505,#3506,#3507));
#1094=EDGE_LOOP('',(#3508,#3509,#3510,#3511));
#1095=EDGE_LOOP('',(#3512,#3513,#3514,#3515));
#1096=EDGE_LOOP('',(#3516,#3517,#3518,#3519));
#1097=EDGE_LOOP('',(#3520,#3521,#3522,#3523,#3524,#3525,#3526));
#1098=EDGE_LOOP('',(#3527));
#1099=EDGE_LOOP('',(#3528));
#1100=EDGE_LOOP('',(#3529,#3530,#3531,#3532));
#1101=EDGE_LOOP('',(#3533));
#1102=EDGE_LOOP('',(#3534,#3535,#3536));
#1103=EDGE_LOOP('',(#3537,#3538,#3539));
#1104=EDGE_LOOP('',(#3540,#3541,#3542));
#1105=EDGE_LOOP('',(#3543,#3544,#3545));
#1106=EDGE_LOOP('',(#3546,#3547,#3548,#3549,#3550,#3551));
#1107=EDGE_LOOP('',(#3552,#3553,#3554,#3555,#3556,#3557));
#1108=EDGE_LOOP('',(#3558,#3559,#3560,#3561,#3562,#3563));
#1109=EDGE_LOOP('',(#3564,#3565,#3566,#3567,#3568,#3569));
#1110=EDGE_LOOP('',(#3570,#3571,#3572,#3573));
#1111=EDGE_LOOP('',(#3574));
#1112=EDGE_LOOP('',(#3575,#3576));
#1113=EDGE_LOOP('',(#3577,#3578,#3579));
#1114=EDGE_LOOP('',(#3580,#3581));
#1115=EDGE_LOOP('',(#3582,#3583));
#1116=EDGE_LOOP('',(#3584,#3585,#3586,#3587));
#1117=EDGE_LOOP('',(#3588,#3589,#3590,#3591));
#1118=EDGE_LOOP('',(#3592,#3593,#3594,#3595));
#1119=EDGE_LOOP('',(#3596,#3597,#3598,#3599));
#1120=EDGE_LOOP('',(#3600,#3601,#3602,#3603));
#1121=EDGE_LOOP('',(#3604,#3605,#3606,#3607,#3608,#3609,#3610,#3611,#3612,
#3613,#3614,#3615));
#1122=EDGE_LOOP('',(#3616));
#1123=EDGE_LOOP('',(#3617,#3618,#3619,#3620));
#1124=EDGE_LOOP('',(#3621,#3622,#3623,#3624));
#1125=EDGE_LOOP('',(#3625,#3626,#3627,#3628));
#1126=EDGE_LOOP('',(#3629,#3630,#3631,#3632));
#1127=EDGE_LOOP('',(#3633,#3634,#3635,#3636));
#1128=EDGE_LOOP('',(#3637,#3638,#3639,#3640));
#1129=EDGE_LOOP('',(#3641,#3642,#3643,#3644));
#1130=EDGE_LOOP('',(#3645,#3646,#3647,#3648));
#1131=EDGE_LOOP('',(#3649,#3650,#3651,#3652));
#1132=EDGE_LOOP('',(#3653,#3654,#3655,#3656));
#1133=EDGE_LOOP('',(#3657,#3658,#3659,#3660));
#1134=EDGE_LOOP('',(#3661,#3662,#3663,#3664));
#1135=EDGE_LOOP('',(#3665,#3666,#3667,#3668));
#1136=EDGE_LOOP('',(#3669,#3670,#3671,#3672));
#1137=EDGE_LOOP('',(#3673,#3674,#3675,#3676));
#1138=EDGE_LOOP('',(#3677));
#1139=EDGE_LOOP('',(#3678));
#1140=EDGE_LOOP('',(#3679));
#1141=EDGE_LOOP('',(#3680));
#1142=EDGE_LOOP('',(#3681,#3682,#3683,#3684));
#1143=EDGE_LOOP('',(#3685,#3686,#3687,#3688));
#1144=EDGE_LOOP('',(#3689,#3690,#3691,#3692));
#1145=EDGE_LOOP('',(#3693,#3694,#3695,#3696));
#1146=EDGE_LOOP('',(#3697,#3698,#3699,#3700));
#1147=EDGE_LOOP('',(#3701,#3702,#3703,#3704));
#1148=EDGE_LOOP('',(#3705,#3706,#3707,#3708));
#1149=EDGE_LOOP('',(#3709,#3710,#3711,#3712));
#1150=EDGE_LOOP('',(#3713,#3714,#3715,#3716));
#1151=EDGE_LOOP('',(#3717,#3718,#3719,#3720));
#1152=EDGE_LOOP('',(#3721,#3722,#3723,#3724));
#1153=EDGE_LOOP('',(#3725,#3726,#3727,#3728));
#1154=EDGE_LOOP('',(#3729,#3730,#3731,#3732,#3733,#3734));
#1155=EDGE_LOOP('',(#3735,#3736,#3737,#3738,#3739,#3740));
#1156=EDGE_LOOP('',(#3741));
#1157=EDGE_LOOP('',(#3742));
#1158=EDGE_LOOP('',(#3743,#3744,#3745,#3746));
#1159=EDGE_LOOP('',(#3747,#3748,#3749,#3750));
#1160=EDGE_LOOP('',(#3751,#3752,#3753,#3754));
#1161=EDGE_LOOP('',(#3755));
#1162=EDGE_LOOP('',(#3756));
#1163=EDGE_LOOP('',(#3757,#3758,#3759,#3760));
#1164=EDGE_LOOP('',(#3761,#3762,#3763,#3764));
#1165=LINE('',#6207,#1473);
#1166=LINE('',#6214,#1474);
#1167=LINE('',#6221,#1475);
#1168=LINE('',#6227,#1476);
#1169=LINE('',#6233,#1477);
#1170=LINE('',#6239,#1478);
#1171=LINE('',#6244,#1479);
#1172=LINE('',#6248,#1480);
#1173=LINE('',#6252,#1481);
#1174=LINE('',#6255,#1482);
#1175=LINE('',#6258,#1483);
#1176=LINE('',#6260,#1484);
#1177=LINE('',#6262,#1485);
#1178=LINE('',#6264,#1486);
#1179=LINE('',#6265,#1487);
#1180=LINE('',#6270,#1488);
#1181=LINE('',#6276,#1489);
#1182=LINE('',#6286,#1490);
#1183=LINE('',#6288,#1491);
#1184=LINE('',#6289,#1492);
#1185=LINE('',#6292,#1493);
#1186=LINE('',#6293,#1494);
#1187=LINE('',#6296,#1495);
#1188=LINE('',#6297,#1496);
#1189=LINE('',#6299,#1497);
#1190=LINE('',#6309,#1498);
#1191=LINE('',#6315,#1499);
#1192=LINE('',#6324,#1500);
#1193=LINE('',#6331,#1501);
#1194=LINE('',#6338,#1502);
#1195=LINE('',#6344,#1503);
#1196=LINE('',#6350,#1504);
#1197=LINE('',#6356,#1505);
#1198=LINE('',#6361,#1506);
#1199=LINE('',#6365,#1507);
#1200=LINE('',#6369,#1508);
#1201=LINE('',#6372,#1509);
#1202=LINE('',#6375,#1510);
#1203=LINE('',#6377,#1511);
#1204=LINE('',#6379,#1512);
#1205=LINE('',#6381,#1513);
#1206=LINE('',#6382,#1514);
#1207=LINE('',#6387,#1515);
#1208=LINE('',#6393,#1516);
#1209=LINE('',#6404,#1517);
#1210=LINE('',#6405,#1518);
#1211=LINE('',#6406,#1519);
#1212=LINE('',#6409,#1520);
#1213=LINE('',#6410,#1521);
#1214=LINE('',#6413,#1522);
#1215=LINE('',#6414,#1523);
#1216=LINE('',#6416,#1524);
#1217=LINE('',#6427,#1525);
#1218=LINE('',#6432,#1526);
#1219=LINE('',#6441,#1527);
#1220=LINE('',#6447,#1528);
#1221=LINE('',#6453,#1529);
#1222=LINE('',#6459,#1530);
#1223=LINE('',#6464,#1531);
#1224=LINE('',#6466,#1532);
#1225=LINE('',#6468,#1533);
#1226=LINE('',#6469,#1534);
#1227=LINE('',#6473,#1535);
#1228=LINE('',#6475,#1536);
#1229=LINE('',#6477,#1537);
#1230=LINE('',#6478,#1538);
#1231=LINE('',#6481,#1539);
#1232=LINE('',#6483,#1540);
#1233=LINE('',#6484,#1541);
#1234=LINE('',#6487,#1542);
#1235=LINE('',#6489,#1543);
#1236=LINE('',#6490,#1544);
#1237=LINE('',#6494,#1545);
#1238=LINE('',#6496,#1546);
#1239=LINE('',#6498,#1547);
#1240=LINE('',#6500,#1548);
#1241=LINE('',#6501,#1549);
#1242=LINE('',#6504,#1550);
#1243=LINE('',#6505,#1551);
#1244=LINE('',#6508,#1552);
#1245=LINE('',#6509,#1553);
#1246=LINE('',#6514,#1554);
#1247=LINE('',#6515,#1555);
#1248=LINE('',#6518,#1556);
#1249=LINE('',#6519,#1557);
#1250=LINE('',#6521,#1558);
#1251=LINE('',#6532,#1559);
#1252=LINE('',#6538,#1560);
#1253=LINE('',#6542,#1561);
#1254=LINE('',#6555,#1562);
#1255=LINE('',#6563,#1563);
#1256=LINE('',#6568,#1564);
#1257=LINE('',#6577,#1565);
#1258=LINE('',#6584,#1566);
#1259=LINE('',#6591,#1567);
#1260=LINE('',#6597,#1568);
#1261=LINE('',#6603,#1569);
#1262=LINE('',#6609,#1570);
#1263=LINE('',#6615,#1571);
#1264=LINE('',#6620,#1572);
#1265=LINE('',#6622,#1573);
#1266=LINE('',#6624,#1574);
#1267=LINE('',#6625,#1575);
#1268=LINE('',#6628,#1576);
#1269=LINE('',#6630,#1577);
#1270=LINE('',#6631,#1578);
#1271=LINE('',#6634,#1579);
#1272=LINE('',#6636,#1580);
#1273=LINE('',#6637,#1581);
#1274=LINE('',#6639,#1582);
#1275=LINE('',#6640,#1583);
#1276=LINE('',#6648,#1584);
#1277=LINE('',#6654,#1585);
#1278=LINE('',#6663,#1586);
#1279=LINE('',#6669,#1587);
#1280=LINE('',#6678,#1588);
#1281=LINE('',#6684,#1589);
#1282=LINE('',#6693,#1590);
#1283=LINE('',#6699,#1591);
#1284=LINE('',#6708,#1592);
#1285=LINE('',#6717,#1593);
#1286=LINE('',#6725,#1594);
#1287=LINE('',#6727,#1595);
#1288=LINE('',#6729,#1596);
#1289=LINE('',#6730,#1597);
#1290=LINE('',#6733,#1598);
#1291=LINE('',#6735,#1599);
#1292=LINE('',#6736,#1600);
#1293=LINE('',#6739,#1601);
#1294=LINE('',#6741,#1602);
#1295=LINE('',#6742,#1603);
#1296=LINE('',#6745,#1604);
#1297=LINE('',#6747,#1605);
#1298=LINE('',#6748,#1606);
#1299=LINE('',#6751,#1607);
#1300=LINE('',#6753,#1608);
#1301=LINE('',#6754,#1609);
#1302=LINE('',#6756,#1610);
#1303=LINE('',#6757,#1611);
#1304=LINE('',#6767,#1612);
#1305=LINE('',#6776,#1613);
#1306=LINE('',#6780,#1614);
#1307=LINE('',#6784,#1615);
#1308=LINE('',#6791,#1616);
#1309=LINE('',#6793,#1617);
#1310=LINE('',#6799,#1618);
#1311=LINE('',#6803,#1619);
#1312=LINE('',#6810,#1620);
#1313=LINE('',#6825,#1621);
#1314=LINE('',#6846,#1622);
#1315=LINE('',#6871,#1623);
#1316=LINE('',#6872,#1624);
#1317=LINE('',#6874,#1625);
#1318=LINE('',#6876,#1626);
#1319=LINE('',#6881,#1627);
#1320=LINE('',#6884,#1628);
#1321=LINE('',#6886,#1629);
#1322=LINE('',#6894,#1630);
#1323=LINE('',#6896,#1631);
#1324=LINE('',#6898,#1632);
#1325=LINE('',#6900,#1633);
#1326=LINE('',#6902,#1634);
#1327=LINE('',#6903,#1635);
#1328=LINE('',#6909,#1636);
#1329=LINE('',#6911,#1637);
#1330=LINE('',#6913,#1638);
#1331=LINE('',#6915,#1639);
#1332=LINE('',#6917,#1640);
#1333=LINE('',#6918,#1641);
#1334=LINE('',#6922,#1642);
#1335=LINE('',#6923,#1643);
#1336=LINE('',#6925,#1644);
#1337=LINE('',#6927,#1645);
#1338=LINE('',#6929,#1646);
#1339=LINE('',#6931,#1647);
#1340=LINE('',#6935,#1648);
#1341=LINE('',#6943,#1649);
#1342=LINE('',#6947,#1650);
#1343=LINE('',#6951,#1651);
#1344=LINE('',#6956,#1652);
#1345=LINE('',#6964,#1653);
#1346=LINE('',#6968,#1654);
#1347=LINE('',#6972,#1655);
#1348=LINE('',#6979,#1656);
#1349=LINE('',#6983,#1657);
#1350=LINE('',#6987,#1658);
#1351=LINE('',#6992,#1659);
#1352=LINE('',#6994,#1660);
#1353=LINE('',#6996,#1661);
#1354=LINE('',#6997,#1662);
#1355=LINE('',#7000,#1663);
#1356=LINE('',#7002,#1664);
#1357=LINE('',#7003,#1665);
#1358=LINE('',#7006,#1666);
#1359=LINE('',#7008,#1667);
#1360=LINE('',#7009,#1668);
#1361=LINE('',#7012,#1669);
#1362=LINE('',#7014,#1670);
#1363=LINE('',#7015,#1671);
#1364=LINE('',#7018,#1672);
#1365=LINE('',#7020,#1673);
#1366=LINE('',#7021,#1674);
#1367=LINE('',#7023,#1675);
#1368=LINE('',#7024,#1676);
#1369=LINE('',#7071,#1677);
#1370=LINE('',#7073,#1678);
#1371=LINE('',#7074,#1679);
#1372=LINE('',#7079,#1680);
#1373=LINE('',#7081,#1681);
#1374=LINE('',#7087,#1682);
#1375=LINE('',#7088,#1683);
#1376=LINE('',#7091,#1684);
#1377=LINE('',#7097,#1685);
#1378=LINE('',#7107,#1686);
#1379=LINE('',#7115,#1687);
#1380=LINE('',#7116,#1688);
#1381=LINE('',#7122,#1689);
#1382=LINE('',#7123,#1690);
#1383=LINE('',#7129,#1691);
#1384=LINE('',#7130,#1692);
#1385=LINE('',#7136,#1693);
#1386=LINE('',#7137,#1694);
#1387=LINE('',#7139,#1695);
#1388=LINE('',#7141,#1696);
#1389=LINE('',#7143,#1697);
#1390=LINE('',#7144,#1698);
#1391=LINE('',#7146,#1699);
#1392=LINE('',#7148,#1700);
#1393=LINE('',#7149,#1701);
#1394=LINE('',#7151,#1702);
#1395=LINE('',#7153,#1703);
#1396=LINE('',#7154,#1704);
#1397=LINE('',#7156,#1705);
#1398=LINE('',#7157,#1706);
#1399=LINE('',#7172,#1707);
#1400=LINE('',#7174,#1708);
#1401=LINE('',#7176,#1709);
#1402=LINE('',#7177,#1710);
#1403=LINE('',#7180,#1711);
#1404=LINE('',#7182,#1712);
#1405=LINE('',#7183,#1713);
#1406=LINE('',#7186,#1714);
#1407=LINE('',#7188,#1715);
#1408=LINE('',#7189,#1716);
#1409=LINE('',#7191,#1717);
#1410=LINE('',#7192,#1718);
#1411=LINE('',#7196,#1719);
#1412=LINE('',#7203,#1720);
#1413=LINE('',#7205,#1721);
#1414=LINE('',#7207,#1722);
#1415=LINE('',#7208,#1723);
#1416=LINE('',#7211,#1724);
#1417=LINE('',#7213,#1725);
#1418=LINE('',#7214,#1726);
#1419=LINE('',#7217,#1727);
#1420=LINE('',#7219,#1728);
#1421=LINE('',#7220,#1729);
#1422=LINE('',#7222,#1730);
#1423=LINE('',#7223,#1731);
#1424=LINE('',#7227,#1732);
#1425=LINE('',#7229,#1733);
#1426=LINE('',#7231,#1734);
#1427=LINE('',#7232,#1735);
#1428=LINE('',#7235,#1736);
#1429=LINE('',#7237,#1737);
#1430=LINE('',#7238,#1738);
#1431=LINE('',#7241,#1739);
#1432=LINE('',#7243,#1740);
#1433=LINE('',#7244,#1741);
#1434=LINE('',#7246,#1742);
#1435=LINE('',#7247,#1743);
#1436=LINE('',#7255,#1744);
#1437=LINE('',#7261,#1745);
#1438=LINE('',#7269,#1746);
#1439=LINE('',#7271,#1747);
#1440=LINE('',#7273,#1748);
#1441=LINE('',#7274,#1749);
#1442=LINE('',#7277,#1750);
#1443=LINE('',#7279,#1751);
#1444=LINE('',#7280,#1752);
#1445=LINE('',#7283,#1753);
#1446=LINE('',#7285,#1754);
#1447=LINE('',#7286,#1755);
#1448=LINE('',#7288,#1756);
#1449=LINE('',#7289,#1757);
#1450=LINE('',#7296,#1758);
#1451=LINE('',#7298,#1759);
#1452=LINE('',#7300,#1760);
#1453=LINE('',#7301,#1761);
#1454=LINE('',#7304,#1762);
#1455=LINE('',#7306,#1763);
#1456=LINE('',#7307,#1764);
#1457=LINE('',#7310,#1765);
#1458=LINE('',#7312,#1766);
#1459=LINE('',#7313,#1767);
#1460=LINE('',#7316,#1768);
#1461=LINE('',#7318,#1769);
#1462=LINE('',#7319,#1770);
#1463=LINE('',#7322,#1771);
#1464=LINE('',#7324,#1772);
#1465=LINE('',#7325,#1773);
#1466=LINE('',#7327,#1774);
#1467=LINE('',#7328,#1775);
#1468=LINE('',#7340,#1776);
#1469=LINE('',#7344,#1777);
#1470=LINE('',#7348,#1778);
#1471=LINE('',#7355,#1779);
#1472=LINE('',#7357,#1780);
#1473=VECTOR('',#4906,0.165);
#1474=VECTOR('',#4915,0.165);
#1475=VECTOR('',#4924,0.275);
#1476=VECTOR('',#4931,0.275);
#1477=VECTOR('',#4938,0.275);
#1478=VECTOR('',#4945,0.275);
#1479=VECTOR('',#4950,1.);
#1480=VECTOR('',#4953,1.);
#1481=VECTOR('',#4958,1.);
#1482=VECTOR('',#4961,1.);
#1483=VECTOR('',#4964,1.);
#1484=VECTOR('',#4965,1.);
#1485=VECTOR('',#4966,1.);
#1486=VECTOR('',#4967,1.);
#1487=VECTOR('',#4968,1.);
#1488=VECTOR('',#4973,0.93);
#1489=VECTOR('',#4980,1.3);
#1490=VECTOR('',#4995,1.);
#1491=VECTOR('',#4996,1.);
#1492=VECTOR('',#4997,1.);
#1493=VECTOR('',#5000,1.);
#1494=VECTOR('',#5001,1.);
#1495=VECTOR('',#5004,1.);
#1496=VECTOR('',#5005,1.);
#1497=VECTOR('',#5008,1.);
#1498=VECTOR('',#5021,0.75);
#1499=VECTOR('',#5028,1.3);
#1500=VECTOR('',#5041,0.165);
#1501=VECTOR('',#5050,0.165);
#1502=VECTOR('',#5059,0.275);
#1503=VECTOR('',#5066,0.275);
#1504=VECTOR('',#5073,0.275);
#1505=VECTOR('',#5080,0.275);
#1506=VECTOR('',#5085,1.);
#1507=VECTOR('',#5088,1.);
#1508=VECTOR('',#5093,1.);
#1509=VECTOR('',#5096,1.);
#1510=VECTOR('',#5099,1.);
#1511=VECTOR('',#5100,1.);
#1512=VECTOR('',#5101,1.);
#1513=VECTOR('',#5102,1.);
#1514=VECTOR('',#5103,1.);
#1515=VECTOR('',#5108,0.93);
#1516=VECTOR('',#5115,1.3);
#1517=VECTOR('',#5130,1.);
#1518=VECTOR('',#5131,1.);
#1519=VECTOR('',#5132,1.);
#1520=VECTOR('',#5135,1.);
#1521=VECTOR('',#5136,1.);
#1522=VECTOR('',#5139,1.);
#1523=VECTOR('',#5140,1.);
#1524=VECTOR('',#5143,1.);
#1525=VECTOR('',#5158,0.75);
#1526=VECTOR('',#5163,1.3);
#1527=VECTOR('',#5176,0.275);
#1528=VECTOR('',#5183,0.275);
#1529=VECTOR('',#5190,0.275);
#1530=VECTOR('',#5197,0.275);
#1531=VECTOR('',#5202,1.);
#1532=VECTOR('',#5203,1.);
#1533=VECTOR('',#5204,1.);
#1534=VECTOR('',#5205,1.);
#1535=VECTOR('',#5208,1.);
#1536=VECTOR('',#5209,1.);
#1537=VECTOR('',#5210,1.);
#1538=VECTOR('',#5211,1.);
#1539=VECTOR('',#5214,1.);
#1540=VECTOR('',#5215,1.);
#1541=VECTOR('',#5216,1.);
#1542=VECTOR('',#5219,1.);
#1543=VECTOR('',#5220,1.);
#1544=VECTOR('',#5221,1.);
#1545=VECTOR('',#5226,1.);
#1546=VECTOR('',#5227,1.);
#1547=VECTOR('',#5228,1.);
#1548=VECTOR('',#5229,1.);
#1549=VECTOR('',#5230,1.);
#1550=VECTOR('',#5233,1.);
#1551=VECTOR('',#5234,1.);
#1552=VECTOR('',#5237,1.);
#1553=VECTOR('',#5238,1.);
#1554=VECTOR('',#5245,1.);
#1555=VECTOR('',#5246,1.);
#1556=VECTOR('',#5249,1.);
#1557=VECTOR('',#5250,1.);
#1558=VECTOR('',#5253,1.);
#1559=VECTOR('',#5268,1.2);
#1560=VECTOR('',#5275,0.405);
#1561=VECTOR('',#5280,0.7);
#1562=VECTOR('',#5299,0.61);
#1563=VECTOR('',#5310,0.405);
#1564=VECTOR('',#5315,1.);
#1565=VECTOR('',#5328,0.3);
#1566=VECTOR('',#5337,0.3);
#1567=VECTOR('',#5346,0.225);
#1568=VECTOR('',#5353,0.225);
#1569=VECTOR('',#5360,0.225);
#1570=VECTOR('',#5367,0.225);
#1571=VECTOR('',#5374,1.01);
#1572=VECTOR('',#5379,1.);
#1573=VECTOR('',#5380,1.);
#1574=VECTOR('',#5381,1.);
#1575=VECTOR('',#5382,1.);
#1576=VECTOR('',#5385,1.);
#1577=VECTOR('',#5386,1.);
#1578=VECTOR('',#5387,1.);
#1579=VECTOR('',#5390,1.);
#1580=VECTOR('',#5391,1.);
#1581=VECTOR('',#5392,1.);
#1582=VECTOR('',#5395,1.);
#1583=VECTOR('',#5396,1.);
#1584=VECTOR('',#5407,0.225);
#1585=VECTOR('',#5414,0.4);
#1586=VECTOR('',#5427,0.225);
#1587=VECTOR('',#5434,0.4);
#1588=VECTOR('',#5447,0.225);
#1589=VECTOR('',#5454,0.4);
#1590=VECTOR('',#5467,0.225);
#1591=VECTOR('',#5474,0.4);
#1592=VECTOR('',#5487,0.3);
#1593=VECTOR('',#5500,0.3);
#1594=VECTOR('',#5511,1.);
#1595=VECTOR('',#5512,1.);
#1596=VECTOR('',#5513,1.);
#1597=VECTOR('',#5514,1.);
#1598=VECTOR('',#5517,1.);
#1599=VECTOR('',#5518,1.);
#1600=VECTOR('',#5519,1.);
#1601=VECTOR('',#5522,1.);
#1602=VECTOR('',#5523,1.);
#1603=VECTOR('',#5524,1.);
#1604=VECTOR('',#5527,1.);
#1605=VECTOR('',#5528,1.);
#1606=VECTOR('',#5529,1.);
#1607=VECTOR('',#5532,1.);
#1608=VECTOR('',#5533,1.);
#1609=VECTOR('',#5534,1.);
#1610=VECTOR('',#5537,1.);
#1611=VECTOR('',#5538,1.);
#1612=VECTOR('',#5551,0.25);
#1613=VECTOR('',#5564,0.4);
#1614=VECTOR('',#5569,0.425);
#1615=VECTOR('',#5574,0.41);
#1616=VECTOR('',#5583,0.26);
#1617=VECTOR('',#5586,0.25);
#1618=VECTOR('',#5593,0.275);
#1619=VECTOR('',#5598,0.265);
#1620=VECTOR('',#5607,0.5);
#1621=VECTOR('',#5616,0.47094010767585);
#1622=VECTOR('',#5623,0.47094010767585);
#1623=VECTOR('',#5626,1.);
#1624=VECTOR('',#5627,1.);
#1625=VECTOR('',#5630,1.);
#1626=VECTOR('',#5633,1.);
#1627=VECTOR('',#5638,0.25);
#1628=VECTOR('',#5643,1.);
#1629=VECTOR('',#5646,1.);
#1630=VECTOR('',#5657,1.);
#1631=VECTOR('',#5658,1.);
#1632=VECTOR('',#5659,1.);
#1633=VECTOR('',#5660,1.);
#1634=VECTOR('',#5661,1.);
#1635=VECTOR('',#5662,1.);
#1636=VECTOR('',#5667,1.);
#1637=VECTOR('',#5668,1.);
#1638=VECTOR('',#5669,1.);
#1639=VECTOR('',#5670,1.);
#1640=VECTOR('',#5671,1.);
#1641=VECTOR('',#5672,1.);
#1642=VECTOR('',#5677,1.);
#1643=VECTOR('',#5678,1.);
#1644=VECTOR('',#5681,1.);
#1645=VECTOR('',#5684,1.);
#1646=VECTOR('',#5687,1.);
#1647=VECTOR('',#5690,1.);
#1648=VECTOR('',#5695,1.065);
#1649=VECTOR('',#5706,1.025);
#1650=VECTOR('',#5711,1.065);
#1651=VECTOR('',#5716,1.025);
#1652=VECTOR('',#5723,0.79);
#1653=VECTOR('',#5734,0.325);
#1654=VECTOR('',#5739,0.35);
#1655=VECTOR('',#5744,0.335);
#1656=VECTOR('',#5753,0.21);
#1657=VECTOR('',#5758,0.2);
#1658=VECTOR('',#5763,0.18);
#1659=VECTOR('',#5768,1.);
#1660=VECTOR('',#5769,1.);
#1661=VECTOR('',#5770,1.);
#1662=VECTOR('',#5771,1.);
#1663=VECTOR('',#5774,1.);
#1664=VECTOR('',#5775,1.);
#1665=VECTOR('',#5776,1.);
#1666=VECTOR('',#5779,1.);
#1667=VECTOR('',#5780,1.);
#1668=VECTOR('',#5781,1.);
#1669=VECTOR('',#5784,1.);
#1670=VECTOR('',#5785,1.);
#1671=VECTOR('',#5786,1.);
#1672=VECTOR('',#5789,1.);
#1673=VECTOR('',#5790,1.);
#1674=VECTOR('',#5791,1.);
#1675=VECTOR('',#5794,1.);
#1676=VECTOR('',#5795,1.);
#1677=VECTOR('',#5882,1.);
#1678=VECTOR('',#5883,1.);
#1679=VECTOR('',#5884,1.);
#1680=VECTOR('',#5889,1.);
#1681=VECTOR('',#5890,1.);
#1682=VECTOR('',#5897,1.);
#1683=VECTOR('',#5898,1.);
#1684=VECTOR('',#5903,1.);
#1685=VECTOR('',#5910,0.75);
#1686=VECTOR('',#5923,0.165);
#1687=VECTOR('',#5932,1.);
#1688=VECTOR('',#5933,1.);
#1689=VECTOR('',#5938,1.);
#1690=VECTOR('',#5939,1.);
#1691=VECTOR('',#5944,1.);
#1692=VECTOR('',#5945,1.);
#1693=VECTOR('',#5950,1.);
#1694=VECTOR('',#5951,1.);
#1695=VECTOR('',#5954,1.);
#1696=VECTOR('',#5955,1.);
#1697=VECTOR('',#5956,1.);
#1698=VECTOR('',#5957,1.);
#1699=VECTOR('',#5960,1.);
#1700=VECTOR('',#5961,1.);
#1701=VECTOR('',#5962,1.);
#1702=VECTOR('',#5965,1.);
#1703=VECTOR('',#5966,1.);
#1704=VECTOR('',#5967,1.);
#1705=VECTOR('',#5970,1.);
#1706=VECTOR('',#5971,1.);
#1707=VECTOR('',#5994,1.);
#1708=VECTOR('',#5995,1.);
#1709=VECTOR('',#5996,1.);
#1710=VECTOR('',#5997,1.);
#1711=VECTOR('',#6000,1.);
#1712=VECTOR('',#6001,1.);
#1713=VECTOR('',#6002,1.);
#1714=VECTOR('',#6005,1.);
#1715=VECTOR('',#6006,1.);
#1716=VECTOR('',#6007,1.);
#1717=VECTOR('',#6010,1.);
#1718=VECTOR('',#6011,1.);
#1719=VECTOR('',#6016,0.4);
#1720=VECTOR('',#6025,1.);
#1721=VECTOR('',#6026,1.);
#1722=VECTOR('',#6027,1.);
#1723=VECTOR('',#6028,1.);
#1724=VECTOR('',#6031,1.);
#1725=VECTOR('',#6032,1.);
#1726=VECTOR('',#6033,1.);
#1727=VECTOR('',#6036,1.);
#1728=VECTOR('',#6037,1.);
#1729=VECTOR('',#6038,1.);
#1730=VECTOR('',#6041,1.);
#1731=VECTOR('',#6042,1.);
#1732=VECTOR('',#6045,1.);
#1733=VECTOR('',#6046,1.);
#1734=VECTOR('',#6047,1.);
#1735=VECTOR('',#6048,1.);
#1736=VECTOR('',#6051,1.);
#1737=VECTOR('',#6052,1.);
#1738=VECTOR('',#6053,1.);
#1739=VECTOR('',#6056,1.);
#1740=VECTOR('',#6057,1.);
#1741=VECTOR('',#6058,1.);
#1742=VECTOR('',#6061,1.);
#1743=VECTOR('',#6062,1.);
#1744=VECTOR('',#6073,0.225);
#1745=VECTOR('',#6080,0.6);
#1746=VECTOR('',#6091,1.);
#1747=VECTOR('',#6092,1.);
#1748=VECTOR('',#6093,1.);
#1749=VECTOR('',#6094,1.);
#1750=VECTOR('',#6097,1.);
#1751=VECTOR('',#6098,1.);
#1752=VECTOR('',#6099,1.);
#1753=VECTOR('',#6102,1.);
#1754=VECTOR('',#6103,1.);
#1755=VECTOR('',#6104,1.);
#1756=VECTOR('',#6107,1.);
#1757=VECTOR('',#6108,1.);
#1758=VECTOR('',#6117,1.);
#1759=VECTOR('',#6118,1.);
#1760=VECTOR('',#6119,1.);
#1761=VECTOR('',#6120,1.);
#1762=VECTOR('',#6123,1.);
#1763=VECTOR('',#6124,1.);
#1764=VECTOR('',#6125,1.);
#1765=VECTOR('',#6128,1.);
#1766=VECTOR('',#6129,1.);
#1767=VECTOR('',#6130,1.);
#1768=VECTOR('',#6133,1.);
#1769=VECTOR('',#6134,1.);
#1770=VECTOR('',#6135,1.);
#1771=VECTOR('',#6138,1.);
#1772=VECTOR('',#6139,1.);
#1773=VECTOR('',#6140,1.);
#1774=VECTOR('',#6143,1.);
#1775=VECTOR('',#6144,1.);
#1776=VECTOR('',#6161,0.325);
#1777=VECTOR('',#6166,0.35);
#1778=VECTOR('',#6171,0.335);
#1779=VECTOR('',#6180,0.21);
#1780=VECTOR('',#6183,0.2);
#1781=CIRCLE('',#4402,0.165);
#1782=CIRCLE('',#4403,0.165);
#1783=CIRCLE('',#4406,0.165);
#1784=CIRCLE('',#4407,0.165);
#1785=CIRCLE('',#4410,0.275);
#1786=CIRCLE('',#4411,0.275);
#1787=CIRCLE('',#4413,0.275);
#1788=CIRCLE('',#4414,0.275);
#1789=CIRCLE('',#4416,0.275);
#1790=CIRCLE('',#4417,0.275);
#1791=CIRCLE('',#4419,0.275);
#1792=CIRCLE('',#4420,0.275);
#1793=CIRCLE('',#4422,0.7);
#1794=CIRCLE('',#4423,0.7);
#1795=CIRCLE('',#4425,0.556776436283003);
#1796=CIRCLE('',#4428,0.93);
#1797=CIRCLE('',#4429,0.93);
#1798=CIRCLE('',#4431,1.3);
#1799=CIRCLE('',#4432,1.3);
#1800=CIRCLE('',#4434,1.24899959967968);
#1801=CIRCLE('',#4437,1.59980467557762);
#1802=CIRCLE('',#4445,1.11803398874989);
#1803=CIRCLE('',#4446,0.75);
#1804=CIRCLE('',#4448,0.75);
#1805=CIRCLE('',#4450,1.3);
#1806=CIRCLE('',#4451,1.3);
#1807=CIRCLE('',#4456,0.165);
#1808=CIRCLE('',#4457,0.165);
#1809=CIRCLE('',#4460,0.165);
#1810=CIRCLE('',#4461,0.165);
#1811=CIRCLE('',#4464,0.275);
#1812=CIRCLE('',#4465,0.275);
#1813=CIRCLE('',#4467,0.275);
#1814=CIRCLE('',#4468,0.275);
#1815=CIRCLE('',#4470,0.275);
#1816=CIRCLE('',#4471,0.275);
#1817=CIRCLE('',#4473,0.275);
#1818=CIRCLE('',#4474,0.275);
#1819=CIRCLE('',#4476,0.7);
#1820=CIRCLE('',#4477,0.7);
#1821=CIRCLE('',#4479,0.556776436283003);
#1822=CIRCLE('',#4482,0.93);
#1823=CIRCLE('',#4483,0.93);
#1824=CIRCLE('',#4485,1.3);
#1825=CIRCLE('',#4486,1.3);
#1826=CIRCLE('',#4489,1.24899959967968);
#1827=CIRCLE('',#4491,1.59980467557762);
#1828=CIRCLE('',#4499,1.11803398874989);
#1829=CIRCLE('',#4500,0.75);
#1830=CIRCLE('',#4502,0.75);
#1831=CIRCLE('',#4504,1.3);
#1832=CIRCLE('',#4505,1.3);
#1833=CIRCLE('',#4510,0.275);
#1834=CIRCLE('',#4511,0.275);
#1835=CIRCLE('',#4513,0.275);
#1836=CIRCLE('',#4514,0.275);
#1837=CIRCLE('',#4516,0.275);
#1838=CIRCLE('',#4517,0.275);
#1839=CIRCLE('',#4519,0.275);
#1840=CIRCLE('',#4520,0.275);
#1841=CIRCLE('',#4526,1.6);
#1842=CIRCLE('',#4530,1.6);
#1843=CIRCLE('',#4537,1.2);
#1844=CIRCLE('',#4538,0.7);
#1845=CIRCLE('',#4540,1.2);
#1846=CIRCLE('',#4542,0.405);
#1847=CIRCLE('',#4544,0.405);
#1848=CIRCLE('',#4546,0.7);
#1849=CIRCLE('',#4550,0.1);
#1850=CIRCLE('',#4551,0.4);
#1851=CIRCLE('',#4554,0.61);
#1852=CIRCLE('',#4555,0.61);
#1853=CIRCLE('',#4557,0.405);
#1854=CIRCLE('',#4559,0.405);
#1855=CIRCLE('',#4561,1.);
#1856=CIRCLE('',#4562,1.);
#1857=CIRCLE('',#4567,0.3);
#1858=CIRCLE('',#4568,0.3);
#1859=CIRCLE('',#4571,0.3);
#1860=CIRCLE('',#4572,0.3);
#1861=CIRCLE('',#4575,0.225);
#1862=CIRCLE('',#4576,0.225);
#1863=CIRCLE('',#4578,0.225);
#1864=CIRCLE('',#4579,0.225);
#1865=CIRCLE('',#4581,0.225);
#1866=CIRCLE('',#4582,0.225);
#1867=CIRCLE('',#4584,0.225);
#1868=CIRCLE('',#4585,0.225);
#1869=CIRCLE('',#4587,1.01);
#1870=CIRCLE('',#4588,1.01);
#1871=CIRCLE('',#4597,0.225);
#1872=CIRCLE('',#4598,0.225);
#1873=CIRCLE('',#4600,0.4);
#1874=CIRCLE('',#4601,0.4);
#1875=CIRCLE('',#4606,0.225);
#1876=CIRCLE('',#4607,0.225);
#1877=CIRCLE('',#4609,0.4);
#1878=CIRCLE('',#4610,0.4);
#1879=CIRCLE('',#4615,0.225);
#1880=CIRCLE('',#4616,0.225);
#1881=CIRCLE('',#4618,0.4);
#1882=CIRCLE('',#4619,0.4);
#1883=CIRCLE('',#4624,0.225);
#1884=CIRCLE('',#4625,0.225);
#1885=CIRCLE('',#4627,0.4);
#1886=CIRCLE('',#4628,0.4);
#1887=CIRCLE('',#4633,0.3);
#1888=CIRCLE('',#4634,0.3);
#1889=CIRCLE('',#4639,0.3);
#1890=CIRCLE('',#4640,0.3);
#1891=CIRCLE('',#4653,0.25);
#1892=CIRCLE('',#4654,0.24505);
#1893=CIRCLE('',#4656,0.25);
#1894=CIRCLE('',#4659,0.375);
#1895=CIRCLE('',#4661,0.425);
#1896=CIRCLE('',#4663,0.425);
#1897=CIRCLE('',#4665,0.395);
#1898=CIRCLE('',#4667,0.27);
#1899=CIRCLE('',#4669,0.24505);
#1900=CIRCLE('',#4673,0.285);
#1901=CIRCLE('',#4674,0.265);
#1902=CIRCLE('',#4676,0.265);
#1903=CIRCLE('',#4678,0.5);
#1904=CIRCLE('',#4680,0.5);
#1905=CIRCLE('',#4684,0.38);
#1906=CIRCLE('',#4686,0.38);
#1907=CIRCLE('',#4691,0.2117);
#1908=CIRCLE('',#4692,0.2117);
#1909=CIRCLE('',#4700,1.065);
#1910=CIRCLE('',#4702,1.065);
#1911=CIRCLE('',#4710,1.065);
#1912=CIRCLE('',#4712,0.985);
#1913=CIRCLE('',#4713,0.79);
#1914=CIRCLE('',#4716,1.065);
#1915=CIRCLE('',#4718,0.985);
#1916=CIRCLE('',#4720,0.79);
#1917=CIRCLE('',#4724,0.3);
#1918=CIRCLE('',#4726,0.35);
#1919=CIRCLE('',#4728,0.35);
#1920=CIRCLE('',#4730,0.32);
#1921=CIRCLE('',#4732,0.22);
#1922=CIRCLE('',#4734,0.1954);
#1923=CIRCLE('',#4736,0.1954);
#1924=CIRCLE('',#4738,0.16);
#1925=CIRCLE('',#4788,1.48592563743951);
#1926=CIRCLE('',#4790,1.48592563743951);
#1927=CIRCLE('',#4791,1.48592563743951);
#1928=CIRCLE('',#4793,1.48592563743951);
#1929=CIRCLE('',#4795,1.48592563743951);
#1930=CIRCLE('',#4798,0.75);
#1931=CIRCLE('',#4799,0.75);
#1932=CIRCLE('',#4801,1.5);
#1933=CIRCLE('',#4804,0.165);
#1934=CIRCLE('',#4805,0.165);
#1935=CIRCLE('',#4808,0.4);
#1936=CIRCLE('',#4810,0.4);
#1937=CIRCLE('',#4812,0.4);
#1938=CIRCLE('',#4814,0.4);
#1939=CIRCLE('',#4821,0.4);
#1940=CIRCLE('',#4823,0.4);
#1941=CIRCLE('',#4824,0.4);
#1942=CIRCLE('',#4826,0.4);
#1943=CIRCLE('',#4828,0.4);
#1944=CIRCLE('',#4835,0.4);
#1945=CIRCLE('',#4850,0.225);
#1946=CIRCLE('',#4851,0.225);
#1947=CIRCLE('',#4853,0.6);
#1948=CIRCLE('',#4854,0.6);
#1949=CIRCLE('',#4874,0.1954);
#1950=CIRCLE('',#4876,0.3);
#1951=CIRCLE('',#4878,0.35);
#1952=CIRCLE('',#4880,0.35);
#1953=CIRCLE('',#4882,0.32);
#1954=CIRCLE('',#4884,0.22);
#1955=CIRCLE('',#4886,0.1954);
#1956=VERTEX_POINT('',#6204);
#1957=VERTEX_POINT('',#6206);
#1958=VERTEX_POINT('',#6211);
#1959=VERTEX_POINT('',#6213);
#1960=VERTEX_POINT('',#6218);
#1961=VERTEX_POINT('',#6220);
#1962=VERTEX_POINT('',#6224);
#1963=VERTEX_POINT('',#6226);
#1964=VERTEX_POINT('',#6230);
#1965=VERTEX_POINT('',#6232);
#1966=VERTEX_POINT('',#6236);
#1967=VERTEX_POINT('',#6238);
#1968=VERTEX_POINT('',#6242);
#1969=VERTEX_POINT('',#6243);
#1970=VERTEX_POINT('',#6245);
#1971=VERTEX_POINT('',#6247);
#1972=VERTEX_POINT('',#6251);
#1973=VERTEX_POINT('',#6253);
#1974=VERTEX_POINT('',#6257);
#1975=VERTEX_POINT('',#6259);
#1976=VERTEX_POINT('',#6261);
#1977=VERTEX_POINT('',#6263);
#1978=VERTEX_POINT('',#6267);
#1979=VERTEX_POINT('',#6269);
#1980=VERTEX_POINT('',#6273);
#1981=VERTEX_POINT('',#6275);
#1982=VERTEX_POINT('',#6279);
#1983=VERTEX_POINT('',#6285);
#1984=VERTEX_POINT('',#6287);
#1985=VERTEX_POINT('',#6291);
#1986=VERTEX_POINT('',#6295);
#1987=VERTEX_POINT('',#6303);
#1988=VERTEX_POINT('',#6305);
#1989=VERTEX_POINT('',#6308);
#1990=VERTEX_POINT('',#6312);
#1991=VERTEX_POINT('',#6314);
#1992=VERTEX_POINT('',#6321);
#1993=VERTEX_POINT('',#6323);
#1994=VERTEX_POINT('',#6328);
#1995=VERTEX_POINT('',#6330);
#1996=VERTEX_POINT('',#6335);
#1997=VERTEX_POINT('',#6337);
#1998=VERTEX_POINT('',#6341);
#1999=VERTEX_POINT('',#6343);
#2000=VERTEX_POINT('',#6347);
#2001=VERTEX_POINT('',#6349);
#2002=VERTEX_POINT('',#6353);
#2003=VERTEX_POINT('',#6355);
#2004=VERTEX_POINT('',#6359);
#2005=VERTEX_POINT('',#6360);
#2006=VERTEX_POINT('',#6362);
#2007=VERTEX_POINT('',#6364);
#2008=VERTEX_POINT('',#6368);
#2009=VERTEX_POINT('',#6370);
#2010=VERTEX_POINT('',#6374);
#2011=VERTEX_POINT('',#6376);
#2012=VERTEX_POINT('',#6378);
#2013=VERTEX_POINT('',#6380);
#2014=VERTEX_POINT('',#6384);
#2015=VERTEX_POINT('',#6386);
#2016=VERTEX_POINT('',#6390);
#2017=VERTEX_POINT('',#6392);
#2018=VERTEX_POINT('',#6397);
#2019=VERTEX_POINT('',#6402);
#2020=VERTEX_POINT('',#6403);
#2021=VERTEX_POINT('',#6408);
#2022=VERTEX_POINT('',#6412);
#2023=VERTEX_POINT('',#6420);
#2024=VERTEX_POINT('',#6422);
#2025=VERTEX_POINT('',#6425);
#2026=VERTEX_POINT('',#6429);
#2027=VERTEX_POINT('',#6431);
#2028=VERTEX_POINT('',#6438);
#2029=VERTEX_POINT('',#6440);
#2030=VERTEX_POINT('',#6444);
#2031=VERTEX_POINT('',#6446);
#2032=VERTEX_POINT('',#6450);
#2033=VERTEX_POINT('',#6452);
#2034=VERTEX_POINT('',#6456);
#2035=VERTEX_POINT('',#6458);
#2036=VERTEX_POINT('',#6462);
#2037=VERTEX_POINT('',#6463);
#2038=VERTEX_POINT('',#6465);
#2039=VERTEX_POINT('',#6467);
#2040=VERTEX_POINT('',#6471);
#2041=VERTEX_POINT('',#6472);
#2042=VERTEX_POINT('',#6474);
#2043=VERTEX_POINT('',#6476);
#2044=VERTEX_POINT('',#6480);
#2045=VERTEX_POINT('',#6482);
#2046=VERTEX_POINT('',#6486);
#2047=VERTEX_POINT('',#6488);
#2048=VERTEX_POINT('',#6493);
#2049=VERTEX_POINT('',#6495);
#2050=VERTEX_POINT('',#6497);
#2051=VERTEX_POINT('',#6499);
#2052=VERTEX_POINT('',#6503);
#2053=VERTEX_POINT('',#6507);
#2054=VERTEX_POINT('',#6513);
#2055=VERTEX_POINT('',#6517);
#2056=VERTEX_POINT('',#6525);
#2057=VERTEX_POINT('',#6527);
#2058=VERTEX_POINT('',#6530);
#2059=VERTEX_POINT('',#6534);
#2060=VERTEX_POINT('',#6537);
#2061=VERTEX_POINT('',#6541);
#2062=VERTEX_POINT('',#6547);
#2063=VERTEX_POINT('',#6552);
#2064=VERTEX_POINT('',#6554);
#2065=VERTEX_POINT('',#6558);
#2066=VERTEX_POINT('',#6561);
#2067=VERTEX_POINT('',#6565);
#2068=VERTEX_POINT('',#6567);
#2069=VERTEX_POINT('',#6574);
#2070=VERTEX_POINT('',#6576);
#2071=VERTEX_POINT('',#6581);
#2072=VERTEX_POINT('',#6583);
#2073=VERTEX_POINT('',#6588);
#2074=VERTEX_POINT('',#6590);
#2075=VERTEX_POINT('',#6594);
#2076=VERTEX_POINT('',#6596);
#2077=VERTEX_POINT('',#6600);
#2078=VERTEX_POINT('',#6602);
#2079=VERTEX_POINT('',#6606);
#2080=VERTEX_POINT('',#6608);
#2081=VERTEX_POINT('',#6612);
#2082=VERTEX_POINT('',#6614);
#2083=VERTEX_POINT('',#6618);
#2084=VERTEX_POINT('',#6619);
#2085=VERTEX_POINT('',#6621);
#2086=VERTEX_POINT('',#6623);
#2087=VERTEX_POINT('',#6627);
#2088=VERTEX_POINT('',#6629);
#2089=VERTEX_POINT('',#6633);
#2090=VERTEX_POINT('',#6635);
#2091=VERTEX_POINT('',#6645);
#2092=VERTEX_POINT('',#6647);
#2093=VERTEX_POINT('',#6651);
#2094=VERTEX_POINT('',#6653);
#2095=VERTEX_POINT('',#6660);
#2096=VERTEX_POINT('',#6662);
#2097=VERTEX_POINT('',#6666);
#2098=VERTEX_POINT('',#6668);
#2099=VERTEX_POINT('',#6675);
#2100=VERTEX_POINT('',#6677);
#2101=VERTEX_POINT('',#6681);
#2102=VERTEX_POINT('',#6683);
#2103=VERTEX_POINT('',#6690);
#2104=VERTEX_POINT('',#6692);
#2105=VERTEX_POINT('',#6696);
#2106=VERTEX_POINT('',#6698);
#2107=VERTEX_POINT('',#6705);
#2108=VERTEX_POINT('',#6707);
#2109=VERTEX_POINT('',#6714);
#2110=VERTEX_POINT('',#6716);
#2111=VERTEX_POINT('',#6723);
#2112=VERTEX_POINT('',#6724);
#2113=VERTEX_POINT('',#6726);
#2114=VERTEX_POINT('',#6728);
#2115=VERTEX_POINT('',#6732);
#2116=VERTEX_POINT('',#6734);
#2117=VERTEX_POINT('',#6738);
#2118=VERTEX_POINT('',#6740);
#2119=VERTEX_POINT('',#6744);
#2120=VERTEX_POINT('',#6746);
#2121=VERTEX_POINT('',#6750);
#2122=VERTEX_POINT('',#6752);
#2123=VERTEX_POINT('',#6761);
#2124=VERTEX_POINT('',#6763);
#2125=VERTEX_POINT('',#6766);
#2126=VERTEX_POINT('',#6771);
#2127=VERTEX_POINT('',#6774);
#2128=VERTEX_POINT('',#6778);
#2129=VERTEX_POINT('',#6782);
#2130=VERTEX_POINT('',#6786);
#2131=VERTEX_POINT('',#6789);
#2132=VERTEX_POINT('',#6796);
#2133=VERTEX_POINT('',#6798);
#2134=VERTEX_POINT('',#6802);
#2135=VERTEX_POINT('',#6806);
#2136=VERTEX_POINT('',#6809);
#2137=VERTEX_POINT('',#6815);
#2138=VERTEX_POINT('',#6816);
#2139=VERTEX_POINT('',#6820);
#2140=VERTEX_POINT('',#6824);
#2141=VERTEX_POINT('',#6827);
#2142=VERTEX_POINT('',#6831);
#2143=VERTEX_POINT('',#6835);
#2144=VERTEX_POINT('',#6843);
#2145=VERTEX_POINT('',#6845);
#2146=VERTEX_POINT('',#6847);
#2147=VERTEX_POINT('',#6851);
#2148=VERTEX_POINT('',#6855);
#2149=VERTEX_POINT('',#6859);
#2150=VERTEX_POINT('',#6863);
#2151=VERTEX_POINT('',#6878);
#2152=VERTEX_POINT('',#6880);
#2153=VERTEX_POINT('',#6892);
#2154=VERTEX_POINT('',#6893);
#2155=VERTEX_POINT('',#6895);
#2156=VERTEX_POINT('',#6897);
#2157=VERTEX_POINT('',#6899);
#2158=VERTEX_POINT('',#6901);
#2159=VERTEX_POINT('',#6904);
#2160=VERTEX_POINT('',#6907);
#2161=VERTEX_POINT('',#6908);
#2162=VERTEX_POINT('',#6910);
#2163=VERTEX_POINT('',#6912);
#2164=VERTEX_POINT('',#6914);
#2165=VERTEX_POINT('',#6916);
#2166=VERTEX_POINT('',#6919);
#2167=VERTEX_POINT('',#6934);
#2168=VERTEX_POINT('',#6938);
#2169=VERTEX_POINT('',#6940);
#2170=VERTEX_POINT('',#6945);
#2171=VERTEX_POINT('',#6949);
#2172=VERTEX_POINT('',#6953);
#2173=VERTEX_POINT('',#6959);
#2174=VERTEX_POINT('',#6962);
#2175=VERTEX_POINT('',#6966);
#2176=VERTEX_POINT('',#6970);
#2177=VERTEX_POINT('',#6974);
#2178=VERTEX_POINT('',#6977);
#2179=VERTEX_POINT('',#6981);
#2180=VERTEX_POINT('',#6985);
#2181=VERTEX_POINT('',#6990);
#2182=VERTEX_POINT('',#6991);
#2183=VERTEX_POINT('',#6993);
#2184=VERTEX_POINT('',#6995);
#2185=VERTEX_POINT('',#6999);
#2186=VERTEX_POINT('',#7001);
#2187=VERTEX_POINT('',#7005);
#2188=VERTEX_POINT('',#7007);
#2189=VERTEX_POINT('',#7011);
#2190=VERTEX_POINT('',#7013);
#2191=VERTEX_POINT('',#7017);
#2192=VERTEX_POINT('',#7019);
#2193=VERTEX_POINT('',#7067);
#2194=VERTEX_POINT('',#7068);
#2195=VERTEX_POINT('',#7070);
#2196=VERTEX_POINT('',#7072);
#2197=VERTEX_POINT('',#7076);
#2198=VERTEX_POINT('',#7078);
#2199=VERTEX_POINT('',#7080);
#2200=VERTEX_POINT('',#7084);
#2201=VERTEX_POINT('',#7086);
#2202=VERTEX_POINT('',#7094);
#2203=VERTEX_POINT('',#7096);
#2204=VERTEX_POINT('',#7100);
#2205=VERTEX_POINT('',#7104);
#2206=VERTEX_POINT('',#7106);
#2207=VERTEX_POINT('',#7111);
#2208=VERTEX_POINT('',#7112);
#2209=VERTEX_POINT('',#7114);
#2210=VERTEX_POINT('',#7118);
#2211=VERTEX_POINT('',#7119);
#2212=VERTEX_POINT('',#7121);
#2213=VERTEX_POINT('',#7125);
#2214=VERTEX_POINT('',#7126);
#2215=VERTEX_POINT('',#7128);
#2216=VERTEX_POINT('',#7132);
#2217=VERTEX_POINT('',#7133);
#2218=VERTEX_POINT('',#7135);
#2219=VERTEX_POINT('',#7140);
#2220=VERTEX_POINT('',#7142);
#2221=VERTEX_POINT('',#7147);
#2222=VERTEX_POINT('',#7152);
#2223=VERTEX_POINT('',#7162);
#2224=VERTEX_POINT('',#7170);
#2225=VERTEX_POINT('',#7171);
#2226=VERTEX_POINT('',#7173);
#2227=VERTEX_POINT('',#7175);
#2228=VERTEX_POINT('',#7179);
#2229=VERTEX_POINT('',#7181);
#2230=VERTEX_POINT('',#7185);
#2231=VERTEX_POINT('',#7187);
#2232=VERTEX_POINT('',#7195);
#2233=VERTEX_POINT('',#7201);
#2234=VERTEX_POINT('',#7202);
#2235=VERTEX_POINT('',#7204);
#2236=VERTEX_POINT('',#7206);
#2237=VERTEX_POINT('',#7210);
#2238=VERTEX_POINT('',#7212);
#2239=VERTEX_POINT('',#7216);
#2240=VERTEX_POINT('',#7218);
#2241=VERTEX_POINT('',#7225);
#2242=VERTEX_POINT('',#7226);
#2243=VERTEX_POINT('',#7228);
#2244=VERTEX_POINT('',#7230);
#2245=VERTEX_POINT('',#7234);
#2246=VERTEX_POINT('',#7236);
#2247=VERTEX_POINT('',#7240);
#2248=VERTEX_POINT('',#7242);
#2249=VERTEX_POINT('',#7252);
#2250=VERTEX_POINT('',#7254);
#2251=VERTEX_POINT('',#7258);
#2252=VERTEX_POINT('',#7260);
#2253=VERTEX_POINT('',#7267);
#2254=VERTEX_POINT('',#7268);
#2255=VERTEX_POINT('',#7270);
#2256=VERTEX_POINT('',#7272);
#2257=VERTEX_POINT('',#7276);
#2258=VERTEX_POINT('',#7278);
#2259=VERTEX_POINT('',#7282);
#2260=VERTEX_POINT('',#7284);
#2261=VERTEX_POINT('',#7294);
#2262=VERTEX_POINT('',#7295);
#2263=VERTEX_POINT('',#7297);
#2264=VERTEX_POINT('',#7299);
#2265=VERTEX_POINT('',#7303);
#2266=VERTEX_POINT('',#7305);
#2267=VERTEX_POINT('',#7309);
#2268=VERTEX_POINT('',#7311);
#2269=VERTEX_POINT('',#7315);
#2270=VERTEX_POINT('',#7317);
#2271=VERTEX_POINT('',#7321);
#2272=VERTEX_POINT('',#7323);
#2273=VERTEX_POINT('',#7332);
#2274=VERTEX_POINT('',#7335);
#2275=VERTEX_POINT('',#7338);
#2276=VERTEX_POINT('',#7342);
#2277=VERTEX_POINT('',#7346);
#2278=VERTEX_POINT('',#7350);
#2279=VERTEX_POINT('',#7353);
#2280=EDGE_CURVE('',#1956,#1956,#1781,.T.);
#2281=EDGE_CURVE('',#1956,#1957,#1165,.T.);
#2282=EDGE_CURVE('',#1957,#1957,#1782,.T.);
#2283=EDGE_CURVE('',#1958,#1958,#1783,.T.);
#2284=EDGE_CURVE('',#1958,#1959,#1166,.T.);
#2285=EDGE_CURVE('',#1959,#1959,#1784,.T.);
#2286=EDGE_CURVE('',#1960,#1960,#1785,.T.);
#2287=EDGE_CURVE('',#1960,#1961,#1167,.T.);
#2288=EDGE_CURVE('',#1961,#1961,#1786,.T.);
#2289=EDGE_CURVE('',#1962,#1962,#1787,.T.);
#2290=EDGE_CURVE('',#1962,#1963,#1168,.T.);
#2291=EDGE_CURVE('',#1963,#1963,#1788,.T.);
#2292=EDGE_CURVE('',#1964,#1964,#1789,.T.);
#2293=EDGE_CURVE('',#1964,#1965,#1169,.T.);
#2294=EDGE_CURVE('',#1965,#1965,#1790,.T.);
#2295=EDGE_CURVE('',#1966,#1966,#1791,.T.);
#2296=EDGE_CURVE('',#1966,#1967,#1170,.T.);
#2297=EDGE_CURVE('',#1967,#1967,#1792,.T.);
#2298=EDGE_CURVE('',#1968,#1969,#1171,.T.);
#2299=EDGE_CURVE('',#1970,#1968,#1793,.T.);
#2300=EDGE_CURVE('',#1971,#1970,#1172,.T.);
#2301=EDGE_CURVE('',#1969,#1971,#1794,.T.);
#2302=EDGE_CURVE('',#1972,#1968,#1173,.T.);
#2303=EDGE_CURVE('',#1973,#1972,#1795,.T.);
#2304=EDGE_CURVE('',#1970,#1973,#1174,.T.);
#2305=EDGE_CURVE('',#1971,#1974,#1175,.T.);
#2306=EDGE_CURVE('',#1974,#1975,#1176,.T.);
#2307=EDGE_CURVE('',#1975,#1976,#1177,.T.);
#2308=EDGE_CURVE('',#1976,#1977,#1178,.T.);
#2309=EDGE_CURVE('',#1977,#1969,#1179,.T.);
#2310=EDGE_CURVE('',#1978,#1978,#1796,.T.);
#2311=EDGE_CURVE('',#1978,#1979,#1180,.T.);
#2312=EDGE_CURVE('',#1979,#1979,#1797,.T.);
#2313=EDGE_CURVE('',#1980,#1980,#1798,.T.);
#2314=EDGE_CURVE('',#1980,#1981,#1181,.T.);
#2315=EDGE_CURVE('',#1981,#1981,#1799,.T.);
#2316=EDGE_CURVE('',#1982,#1982,#1800,.T.);
#2317=EDGE_CURVE('',#1973,#1972,#1801,.T.);
#2318=EDGE_CURVE('',#1983,#1977,#1182,.T.);
#2319=EDGE_CURVE('',#1983,#1984,#1183,.T.);
#2320=EDGE_CURVE('',#1984,#1974,#1184,.T.);
#2321=EDGE_CURVE('',#1985,#1983,#1185,.T.);
#2322=EDGE_CURVE('',#1985,#1976,#1186,.T.);
#2323=EDGE_CURVE('',#1986,#1985,#1187,.T.);
#2324=EDGE_CURVE('',#1986,#1975,#1188,.T.);
#2325=EDGE_CURVE('',#1984,#1986,#1189,.T.);
#2326=EDGE_CURVE('',#1987,#1987,#1802,.T.);
#2327=EDGE_CURVE('',#1988,#1988,#1803,.T.);
#2328=EDGE_CURVE('',#1988,#1989,#1190,.T.);
#2329=EDGE_CURVE('',#1989,#1989,#1804,.T.);
#2330=EDGE_CURVE('',#1990,#1990,#1805,.T.);
#2331=EDGE_CURVE('',#1990,#1991,#1191,.T.);
#2332=EDGE_CURVE('',#1991,#1991,#1806,.T.);
#2333=EDGE_CURVE('',#1992,#1992,#1807,.T.);
#2334=EDGE_CURVE('',#1992,#1993,#1192,.T.);
#2335=EDGE_CURVE('',#1993,#1993,#1808,.T.);
#2336=EDGE_CURVE('',#1994,#1994,#1809,.T.);
#2337=EDGE_CURVE('',#1994,#1995,#1193,.T.);
#2338=EDGE_CURVE('',#1995,#1995,#1810,.T.);
#2339=EDGE_CURVE('',#1996,#1996,#1811,.T.);
#2340=EDGE_CURVE('',#1996,#1997,#1194,.T.);
#2341=EDGE_CURVE('',#1997,#1997,#1812,.T.);
#2342=EDGE_CURVE('',#1998,#1998,#1813,.T.);
#2343=EDGE_CURVE('',#1998,#1999,#1195,.T.);
#2344=EDGE_CURVE('',#1999,#1999,#1814,.T.);
#2345=EDGE_CURVE('',#2000,#2000,#1815,.T.);
#2346=EDGE_CURVE('',#2000,#2001,#1196,.T.);
#2347=EDGE_CURVE('',#2001,#2001,#1816,.T.);
#2348=EDGE_CURVE('',#2002,#2002,#1817,.T.);
#2349=EDGE_CURVE('',#2002,#2003,#1197,.T.);
#2350=EDGE_CURVE('',#2003,#2003,#1818,.T.);
#2351=EDGE_CURVE('',#2004,#2005,#1198,.T.);
#2352=EDGE_CURVE('',#2006,#2004,#1819,.T.);
#2353=EDGE_CURVE('',#2007,#2006,#1199,.T.);
#2354=EDGE_CURVE('',#2005,#2007,#1820,.T.);
#2355=EDGE_CURVE('',#2008,#2004,#1200,.T.);
#2356=EDGE_CURVE('',#2009,#2008,#1821,.T.);
#2357=EDGE_CURVE('',#2006,#2009,#1201,.T.);
#2358=EDGE_CURVE('',#2007,#2010,#1202,.T.);
#2359=EDGE_CURVE('',#2010,#2011,#1203,.T.);
#2360=EDGE_CURVE('',#2011,#2012,#1204,.T.);
#2361=EDGE_CURVE('',#2012,#2013,#1205,.T.);
#2362=EDGE_CURVE('',#2013,#2005,#1206,.T.);
#2363=EDGE_CURVE('',#2014,#2014,#1822,.T.);
#2364=EDGE_CURVE('',#2014,#2015,#1207,.T.);
#2365=EDGE_CURVE('',#2015,#2015,#1823,.T.);
#2366=EDGE_CURVE('',#2016,#2016,#1824,.T.);
#2367=EDGE_CURVE('',#2016,#2017,#1208,.T.);
#2368=EDGE_CURVE('',#2017,#2017,#1825,.T.);
#2369=EDGE_CURVE('',#2018,#2018,#1826,.T.);
#2370=EDGE_CURVE('',#2009,#2008,#1827,.T.);
#2371=EDGE_CURVE('',#2019,#2020,#1209,.T.);
#2372=EDGE_CURVE('',#2020,#2012,#1210,.T.);
#2373=EDGE_CURVE('',#2019,#2011,#1211,.T.);
#2374=EDGE_CURVE('',#2021,#2019,#1212,.T.);
#2375=EDGE_CURVE('',#2021,#2010,#1213,.T.);
#2376=EDGE_CURVE('',#2022,#2013,#1214,.T.);
#2377=EDGE_CURVE('',#2022,#2021,#1215,.T.);
#2378=EDGE_CURVE('',#2020,#2022,#1216,.T.);
#2379=EDGE_CURVE('',#2023,#2023,#1828,.T.);
#2380=EDGE_CURVE('',#2024,#2024,#1829,.T.);
#2381=EDGE_CURVE('',#2025,#2025,#1830,.T.);
#2382=EDGE_CURVE('',#2025,#2024,#1217,.T.);
#2383=EDGE_CURVE('',#2026,#2026,#1831,.T.);
#2384=EDGE_CURVE('',#2026,#2027,#1218,.T.);
#2385=EDGE_CURVE('',#2027,#2027,#1832,.T.);
#2386=EDGE_CURVE('',#2028,#2028,#1833,.T.);
#2387=EDGE_CURVE('',#2028,#2029,#1219,.T.);
#2388=EDGE_CURVE('',#2029,#2029,#1834,.T.);
#2389=EDGE_CURVE('',#2030,#2030,#1835,.T.);
#2390=EDGE_CURVE('',#2030,#2031,#1220,.T.);
#2391=EDGE_CURVE('',#2031,#2031,#1836,.T.);
#2392=EDGE_CURVE('',#2032,#2032,#1837,.T.);
#2393=EDGE_CURVE('',#2032,#2033,#1221,.T.);
#2394=EDGE_CURVE('',#2033,#2033,#1838,.T.);
#2395=EDGE_CURVE('',#2034,#2034,#1839,.T.);
#2396=EDGE_CURVE('',#2034,#2035,#1222,.T.);
#2397=EDGE_CURVE('',#2035,#2035,#1840,.T.);
#2398=EDGE_CURVE('',#2036,#2037,#1223,.T.);
#2399=EDGE_CURVE('',#2036,#2038,#1224,.T.);
#2400=EDGE_CURVE('',#2039,#2038,#1225,.T.);
#2401=EDGE_CURVE('',#2037,#2039,#1226,.T.);
#2402=EDGE_CURVE('',#2040,#2041,#1227,.T.);
#2403=EDGE_CURVE('',#2040,#2042,#1228,.T.);
#2404=EDGE_CURVE('',#2043,#2042,#1229,.T.);
#2405=EDGE_CURVE('',#2041,#2043,#1230,.T.);
#2406=EDGE_CURVE('',#2044,#2036,#1231,.T.);
#2407=EDGE_CURVE('',#2045,#2044,#1232,.T.);
#2408=EDGE_CURVE('',#2038,#2045,#1233,.T.);
#2409=EDGE_CURVE('',#2046,#2040,#1234,.T.);
#2410=EDGE_CURVE('',#2047,#2046,#1235,.T.);
#2411=EDGE_CURVE('',#2042,#2047,#1236,.T.);
#2412=EDGE_CURVE('',#2045,#2043,#1841,.T.);
#2413=EDGE_CURVE('',#2047,#2048,#1237,.T.);
#2414=EDGE_CURVE('',#2048,#2049,#1238,.T.);
#2415=EDGE_CURVE('',#2049,#2050,#1239,.T.);
#2416=EDGE_CURVE('',#2050,#2051,#1240,.T.);
#2417=EDGE_CURVE('',#2051,#2039,#1241,.T.);
#2418=EDGE_CURVE('',#2052,#2046,#1242,.T.);
#2419=EDGE_CURVE('',#2052,#2048,#1243,.T.);
#2420=EDGE_CURVE('',#2053,#2051,#1244,.T.);
#2421=EDGE_CURVE('',#2037,#2053,#1245,.T.);
#2422=EDGE_CURVE('',#2041,#2044,#1842,.T.);
#2423=EDGE_CURVE('',#2053,#2054,#1246,.T.);
#2424=EDGE_CURVE('',#2054,#2050,#1247,.T.);
#2425=EDGE_CURVE('',#2054,#2055,#1248,.T.);
#2426=EDGE_CURVE('',#2055,#2049,#1249,.T.);
#2427=EDGE_CURVE('',#2055,#2052,#1250,.T.);
#2428=EDGE_CURVE('',#2056,#2056,#1843,.T.);
#2429=EDGE_CURVE('',#2057,#2057,#1844,.T.);
#2430=EDGE_CURVE('',#2058,#2058,#1845,.T.);
#2431=EDGE_CURVE('',#2058,#2056,#1251,.T.);
#2432=EDGE_CURVE('',#2059,#2059,#1846,.T.);
#2433=EDGE_CURVE('',#2059,#2060,#1252,.T.);
#2434=EDGE_CURVE('',#2060,#2060,#1847,.T.);
#2435=EDGE_CURVE('',#2057,#2061,#1253,.T.);
#2436=EDGE_CURVE('',#2061,#2061,#1848,.T.);
#2437=EDGE_CURVE('',#2062,#2062,#1849,.T.);
#2438=EDGE_CURVE('',#2062,#2062,#1850,.T.);
#2439=EDGE_CURVE('',#2063,#2063,#1851,.T.);
#2440=EDGE_CURVE('',#2063,#2064,#1254,.T.);
#2441=EDGE_CURVE('',#2064,#2064,#1852,.T.);
#2442=EDGE_CURVE('',#2065,#2065,#1853,.T.);
#2443=EDGE_CURVE('',#2066,#2066,#1854,.T.);
#2444=EDGE_CURVE('',#2066,#2065,#1255,.T.);
#2445=EDGE_CURVE('',#2067,#2067,#1855,.T.);
#2446=EDGE_CURVE('',#2067,#2068,#1256,.T.);
#2447=EDGE_CURVE('',#2068,#2068,#1856,.T.);
#2448=EDGE_CURVE('',#2069,#2069,#1857,.T.);
#2449=EDGE_CURVE('',#2069,#2070,#1257,.T.);
#2450=EDGE_CURVE('',#2070,#2070,#1858,.T.);
#2451=EDGE_CURVE('',#2071,#2071,#1859,.T.);
#2452=EDGE_CURVE('',#2071,#2072,#1258,.T.);
#2453=EDGE_CURVE('',#2072,#2072,#1860,.T.);
#2454=EDGE_CURVE('',#2073,#2073,#1861,.T.);
#2455=EDGE_CURVE('',#2073,#2074,#1259,.T.);
#2456=EDGE_CURVE('',#2074,#2074,#1862,.T.);
#2457=EDGE_CURVE('',#2075,#2075,#1863,.T.);
#2458=EDGE_CURVE('',#2075,#2076,#1260,.T.);
#2459=EDGE_CURVE('',#2076,#2076,#1864,.T.);
#2460=EDGE_CURVE('',#2077,#2077,#1865,.T.);
#2461=EDGE_CURVE('',#2077,#2078,#1261,.T.);
#2462=EDGE_CURVE('',#2078,#2078,#1866,.T.);
#2463=EDGE_CURVE('',#2079,#2079,#1867,.T.);
#2464=EDGE_CURVE('',#2079,#2080,#1262,.T.);
#2465=EDGE_CURVE('',#2080,#2080,#1868,.T.);
#2466=EDGE_CURVE('',#2081,#2081,#1869,.T.);
#2467=EDGE_CURVE('',#2081,#2082,#1263,.T.);
#2468=EDGE_CURVE('',#2082,#2082,#1870,.T.);
#2469=EDGE_CURVE('',#2083,#2084,#1264,.T.);
#2470=EDGE_CURVE('',#2084,#2085,#1265,.T.);
#2471=EDGE_CURVE('',#2086,#2085,#1266,.T.);
#2472=EDGE_CURVE('',#2083,#2086,#1267,.T.);
#2473=EDGE_CURVE('',#2087,#2083,#1268,.T.);
#2474=EDGE_CURVE('',#2088,#2086,#1269,.T.);
#2475=EDGE_CURVE('',#2087,#2088,#1270,.T.);
#2476=EDGE_CURVE('',#2089,#2087,#1271,.T.);
#2477=EDGE_CURVE('',#2090,#2088,#1272,.T.);
#2478=EDGE_CURVE('',#2089,#2090,#1273,.T.);
#2479=EDGE_CURVE('',#2084,#2089,#1274,.T.);
#2480=EDGE_CURVE('',#2085,#2090,#1275,.T.);
#2481=EDGE_CURVE('',#2091,#2091,#1871,.T.);
#2482=EDGE_CURVE('',#2091,#2092,#1276,.T.);
#2483=EDGE_CURVE('',#2092,#2092,#1872,.T.);
#2484=EDGE_CURVE('',#2093,#2093,#1873,.T.);
#2485=EDGE_CURVE('',#2093,#2094,#1277,.T.);
#2486=EDGE_CURVE('',#2094,#2094,#1874,.T.);
#2487=EDGE_CURVE('',#2095,#2095,#1875,.T.);
#2488=EDGE_CURVE('',#2095,#2096,#1278,.T.);
#2489=EDGE_CURVE('',#2096,#2096,#1876,.T.);
#2490=EDGE_CURVE('',#2097,#2097,#1877,.T.);
#2491=EDGE_CURVE('',#2097,#2098,#1279,.T.);
#2492=EDGE_CURVE('',#2098,#2098,#1878,.T.);
#2493=EDGE_CURVE('',#2099,#2099,#1879,.T.);
#2494=EDGE_CURVE('',#2099,#2100,#1280,.T.);
#2495=EDGE_CURVE('',#2100,#2100,#1880,.T.);
#2496=EDGE_CURVE('',#2101,#2101,#1881,.T.);
#2497=EDGE_CURVE('',#2101,#2102,#1281,.T.);
#2498=EDGE_CURVE('',#2102,#2102,#1882,.T.);
#2499=EDGE_CURVE('',#2103,#2103,#1883,.T.);
#2500=EDGE_CURVE('',#2103,#2104,#1282,.T.);
#2501=EDGE_CURVE('',#2104,#2104,#1884,.T.);
#2502=EDGE_CURVE('',#2105,#2105,#1885,.T.);
#2503=EDGE_CURVE('',#2105,#2106,#1283,.T.);
#2504=EDGE_CURVE('',#2106,#2106,#1886,.T.);
#2505=EDGE_CURVE('',#2107,#2107,#1887,.T.);
#2506=EDGE_CURVE('',#2107,#2108,#1284,.T.);
#2507=EDGE_CURVE('',#2108,#2108,#1888,.T.);
#2508=EDGE_CURVE('',#2109,#2109,#1889,.T.);
#2509=EDGE_CURVE('',#2109,#2110,#1285,.T.);
#2510=EDGE_CURVE('',#2110,#2110,#1890,.T.);
#2511=EDGE_CURVE('',#2111,#2112,#1286,.T.);
#2512=EDGE_CURVE('',#2112,#2113,#1287,.T.);
#2513=EDGE_CURVE('',#2113,#2114,#1288,.T.);
#2514=EDGE_CURVE('',#2111,#2114,#1289,.T.);
#2515=EDGE_CURVE('',#2112,#2115,#1290,.T.);
#2516=EDGE_CURVE('',#2115,#2116,#1291,.T.);
#2517=EDGE_CURVE('',#2116,#2113,#1292,.T.);
#2518=EDGE_CURVE('',#2115,#2117,#1293,.T.);
#2519=EDGE_CURVE('',#2117,#2118,#1294,.T.);
#2520=EDGE_CURVE('',#2118,#2116,#1295,.T.);
#2521=EDGE_CURVE('',#2117,#2119,#1296,.T.);
#2522=EDGE_CURVE('',#2119,#2120,#1297,.T.);
#2523=EDGE_CURVE('',#2120,#2118,#1298,.T.);
#2524=EDGE_CURVE('',#2119,#2121,#1299,.T.);
#2525=EDGE_CURVE('',#2121,#2122,#1300,.T.);
#2526=EDGE_CURVE('',#2122,#2120,#1301,.T.);
#2527=EDGE_CURVE('',#2121,#2111,#1302,.T.);
#2528=EDGE_CURVE('',#2114,#2122,#1303,.T.);
#2529=EDGE_CURVE('',#2123,#2123,#1891,.T.);
#2530=EDGE_CURVE('',#2124,#2124,#1892,.T.);
#2531=EDGE_CURVE('',#2123,#2125,#1304,.T.);
#2532=EDGE_CURVE('',#2125,#2125,#1893,.T.);
#2533=EDGE_CURVE('',#2126,#2126,#1894,.T.);
#2534=EDGE_CURVE('',#2127,#2127,#1895,.T.);
#2535=EDGE_CURVE('',#2127,#2126,#1305,.T.);
#2536=EDGE_CURVE('',#2128,#2128,#1896,.T.);
#2537=EDGE_CURVE('',#2128,#2127,#1306,.T.);
#2538=EDGE_CURVE('',#2129,#2129,#1897,.T.);
#2539=EDGE_CURVE('',#2129,#2128,#1307,.T.);
#2540=EDGE_CURVE('',#2130,#2130,#1898,.T.);
#2541=EDGE_CURVE('',#2131,#2131,#1899,.F.);
#2542=EDGE_CURVE('',#2131,#2130,#1308,.T.);
#2543=EDGE_CURVE('',#2124,#2131,#1309,.T.);
#2544=EDGE_CURVE('',#2132,#2132,#1900,.T.);
#2545=EDGE_CURVE('',#2132,#2133,#1310,.T.);
#2546=EDGE_CURVE('',#2133,#2133,#1901,.T.);
#2547=EDGE_CURVE('',#2133,#2134,#1311,.T.);
#2548=EDGE_CURVE('',#2134,#2134,#1902,.T.);
#2549=EDGE_CURVE('',#2135,#2135,#1903,.T.);
#2550=EDGE_CURVE('',#2135,#2136,#1312,.T.);
#2551=EDGE_CURVE('',#2136,#2136,#1904,.T.);
#2552=EDGE_CURVE('',#2137,#2138,#191,.T.);
#2553=EDGE_CURVE('',#2139,#2137,#192,.T.);
#2554=EDGE_CURVE('',#2139,#2140,#1313,.T.);
#2555=EDGE_CURVE('',#2140,#2140,#1905,.T.);
#2556=EDGE_CURVE('',#2141,#2139,#193,.T.);
#2557=EDGE_CURVE('',#2142,#2141,#194,.T.);
#2558=EDGE_CURVE('',#2143,#2142,#195,.T.);
#2559=EDGE_CURVE('',#2138,#2143,#196,.T.);
#2560=EDGE_CURVE('',#2144,#2144,#1906,.T.);
#2561=EDGE_CURVE('',#2144,#2145,#1314,.T.);
#2562=EDGE_CURVE('',#2146,#2145,#197,.T.);
#2563=EDGE_CURVE('',#2147,#2146,#198,.T.);
#2564=EDGE_CURVE('',#2148,#2147,#199,.T.);
#2565=EDGE_CURVE('',#2149,#2148,#200,.T.);
#2566=EDGE_CURVE('',#2150,#2149,#201,.T.);
#2567=EDGE_CURVE('',#2145,#2150,#202,.T.);
#2568=EDGE_CURVE('',#2141,#2150,#1315,.T.);
#2569=EDGE_CURVE('',#2142,#2149,#1316,.T.);
#2570=EDGE_CURVE('',#2139,#2145,#1317,.T.);
#2571=EDGE_CURVE('',#2137,#2146,#1318,.T.);
#2572=EDGE_CURVE('',#2151,#2151,#1907,.F.);
#2573=EDGE_CURVE('',#2151,#2152,#1319,.T.);
#2574=EDGE_CURVE('',#2152,#2152,#1908,.F.);
#2575=EDGE_CURVE('',#2138,#2147,#1320,.T.);
#2576=EDGE_CURVE('',#2143,#2148,#1321,.T.);
#2577=EDGE_CURVE('',#2153,#2154,#1322,.T.);
#2578=EDGE_CURVE('',#2154,#2155,#1323,.T.);
#2579=EDGE_CURVE('',#2155,#2156,#1324,.T.);
#2580=EDGE_CURVE('',#2156,#2157,#1325,.T.);
#2581=EDGE_CURVE('',#2157,#2158,#1326,.T.);
#2582=EDGE_CURVE('',#2158,#2153,#1327,.T.);
#2583=EDGE_CURVE('',#2159,#2159,#1909,.T.);
#2584=EDGE_CURVE('',#2160,#2161,#1328,.T.);
#2585=EDGE_CURVE('',#2161,#2162,#1329,.T.);
#2586=EDGE_CURVE('',#2162,#2163,#1330,.T.);
#2587=EDGE_CURVE('',#2163,#2164,#1331,.T.);
#2588=EDGE_CURVE('',#2164,#2165,#1332,.T.);
#2589=EDGE_CURVE('',#2165,#2160,#1333,.T.);
#2590=EDGE_CURVE('',#2166,#2166,#1910,.T.);
#2591=EDGE_CURVE('',#2160,#2154,#1334,.T.);
#2592=EDGE_CURVE('',#2155,#2165,#1335,.T.);
#2593=EDGE_CURVE('',#2156,#2164,#1336,.T.);
#2594=EDGE_CURVE('',#2157,#2163,#1337,.T.);
#2595=EDGE_CURVE('',#2158,#2162,#1338,.T.);
#2596=EDGE_CURVE('',#2153,#2161,#1339,.T.);
#2597=EDGE_CURVE('',#2166,#2167,#1340,.T.);
#2598=EDGE_CURVE('',#2167,#2167,#1911,.T.);
#2599=EDGE_CURVE('',#2168,#2168,#1912,.T.);
#2600=EDGE_CURVE('',#2169,#2169,#1913,.T.);
#2601=EDGE_CURVE('',#2167,#2168,#1341,.T.);
#2602=EDGE_CURVE('',#2170,#2170,#1914,.T.);
#2603=EDGE_CURVE('',#2170,#2159,#1342,.T.);
#2604=EDGE_CURVE('',#2171,#2171,#1915,.T.);
#2605=EDGE_CURVE('',#2171,#2170,#1343,.T.);
#2606=EDGE_CURVE('',#2172,#2172,#1916,.T.);
#2607=EDGE_CURVE('',#2172,#2169,#1344,.T.);
#2608=EDGE_CURVE('',#2173,#2173,#1917,.T.);
#2609=EDGE_CURVE('',#2174,#2174,#1918,.T.);
#2610=EDGE_CURVE('',#2174,#2173,#1345,.T.);
#2611=EDGE_CURVE('',#2175,#2175,#1919,.T.);
#2612=EDGE_CURVE('',#2175,#2174,#1346,.T.);
#2613=EDGE_CURVE('',#2176,#2176,#1920,.T.);
#2614=EDGE_CURVE('',#2176,#2175,#1347,.T.);
#2615=EDGE_CURVE('',#2177,#2177,#1921,.T.);
#2616=EDGE_CURVE('',#2178,#2178,#1922,.F.);
#2617=EDGE_CURVE('',#2178,#2177,#1348,.T.);
#2618=EDGE_CURVE('',#2179,#2179,#1923,.F.);
#2619=EDGE_CURVE('',#2179,#2178,#1349,.T.);
#2620=EDGE_CURVE('',#2180,#2180,#1924,.T.);
#2621=EDGE_CURVE('',#2180,#2179,#1350,.T.);
#2622=EDGE_CURVE('',#2181,#2182,#1351,.T.);
#2623=EDGE_CURVE('',#2182,#2183,#1352,.T.);
#2624=EDGE_CURVE('',#2183,#2184,#1353,.T.);
#2625=EDGE_CURVE('',#2181,#2184,#1354,.T.);
#2626=EDGE_CURVE('',#2182,#2185,#1355,.T.);
#2627=EDGE_CURVE('',#2185,#2186,#1356,.T.);
#2628=EDGE_CURVE('',#2186,#2183,#1357,.T.);
#2629=EDGE_CURVE('',#2185,#2187,#1358,.T.);
#2630=EDGE_CURVE('',#2187,#2188,#1359,.T.);
#2631=EDGE_CURVE('',#2188,#2186,#1360,.T.);
#2632=EDGE_CURVE('',#2187,#2189,#1361,.T.);
#2633=EDGE_CURVE('',#2189,#2190,#1362,.T.);
#2634=EDGE_CURVE('',#2190,#2188,#1363,.T.);
#2635=EDGE_CURVE('',#2189,#2191,#1364,.T.);
#2636=EDGE_CURVE('',#2191,#2192,#1365,.T.);
#2637=EDGE_CURVE('',#2192,#2190,#1366,.T.);
#2638=EDGE_CURVE('',#2191,#2181,#1367,.T.);
#2639=EDGE_CURVE('',#2184,#2192,#1368,.T.);
#2640=EDGE_CURVE('',#2193,#2194,#1925,.T.);
#2641=EDGE_CURVE('',#2195,#2193,#1369,.T.);
#2642=EDGE_CURVE('',#2196,#2195,#1370,.T.);
#2643=EDGE_CURVE('',#2196,#2194,#1371,.T.);
#2644=EDGE_CURVE('',#2194,#2197,#1926,.T.);
#2645=EDGE_CURVE('',#2198,#2196,#1372,.T.);
#2646=EDGE_CURVE('',#2198,#2199,#1373,.T.);
#2647=EDGE_CURVE('',#2197,#2199,#1927,.T.);
#2648=EDGE_CURVE('',#2199,#2200,#1928,.T.);
#2649=EDGE_CURVE('',#2201,#2198,#1374,.T.);
#2650=EDGE_CURVE('',#2201,#2200,#1375,.T.);
#2651=EDGE_CURVE('',#2200,#2193,#1929,.T.);
#2652=EDGE_CURVE('',#2195,#2201,#1376,.T.);
#2653=EDGE_CURVE('',#2202,#2202,#1930,.T.);
#2654=EDGE_CURVE('',#2202,#2203,#1377,.T.);
#2655=EDGE_CURVE('',#2203,#2203,#1931,.T.);
#2656=EDGE_CURVE('',#2197,#2204,#1932,.T.);
#2657=EDGE_CURVE('',#2205,#2205,#1933,.T.);
#2658=EDGE_CURVE('',#2205,#2206,#1378,.T.);
#2659=EDGE_CURVE('',#2206,#2206,#1934,.T.);
#2660=EDGE_CURVE('',#2207,#2208,#1935,.T.);
#2661=EDGE_CURVE('',#2209,#2208,#1379,.T.);
#2662=EDGE_CURVE('',#2207,#2209,#1380,.T.);
#2663=EDGE_CURVE('',#2210,#2211,#1936,.T.);
#2664=EDGE_CURVE('',#2212,#2211,#1381,.T.);
#2665=EDGE_CURVE('',#2210,#2212,#1382,.T.);
#2666=EDGE_CURVE('',#2213,#2214,#1937,.T.);
#2667=EDGE_CURVE('',#2215,#2214,#1383,.T.);
#2668=EDGE_CURVE('',#2213,#2215,#1384,.T.);
#2669=EDGE_CURVE('',#2216,#2217,#1938,.T.);
#2670=EDGE_CURVE('',#2218,#2217,#1385,.T.);
#2671=EDGE_CURVE('',#2216,#2218,#1386,.T.);
#2672=EDGE_CURVE('',#2207,#2217,#1387,.T.);
#2673=EDGE_CURVE('',#2209,#2219,#1388,.T.);
#2674=EDGE_CURVE('',#2220,#2219,#1389,.T.);
#2675=EDGE_CURVE('',#2218,#2220,#1390,.T.);
#2676=EDGE_CURVE('',#2216,#2214,#1391,.T.);
#2677=EDGE_CURVE('',#2221,#2220,#1392,.T.);
#2678=EDGE_CURVE('',#2215,#2221,#1393,.T.);
#2679=EDGE_CURVE('',#2213,#2211,#1394,.T.);
#2680=EDGE_CURVE('',#2222,#2221,#1395,.T.);
#2681=EDGE_CURVE('',#2212,#2222,#1396,.T.);
#2682=EDGE_CURVE('',#2210,#2208,#1397,.T.);
#2683=EDGE_CURVE('',#2219,#2222,#1398,.T.);
#2684=EDGE_CURVE('',#2211,#2213,#1939,.T.);
#2685=EDGE_CURVE('',#2208,#2223,#1940,.T.);
#2686=EDGE_CURVE('',#2223,#2210,#1941,.T.);
#2687=EDGE_CURVE('',#2217,#2207,#1942,.T.);
#2688=EDGE_CURVE('',#2214,#2216,#1943,.T.);
#2689=EDGE_CURVE('',#2224,#2225,#1399,.T.);
#2690=EDGE_CURVE('',#2225,#2226,#1400,.T.);
#2691=EDGE_CURVE('',#2227,#2226,#1401,.T.);
#2692=EDGE_CURVE('',#2224,#2227,#1402,.T.);
#2693=EDGE_CURVE('',#2228,#2224,#1403,.T.);
#2694=EDGE_CURVE('',#2229,#2227,#1404,.T.);
#2695=EDGE_CURVE('',#2228,#2229,#1405,.T.);
#2696=EDGE_CURVE('',#2230,#2228,#1406,.T.);
#2697=EDGE_CURVE('',#2231,#2229,#1407,.T.);
#2698=EDGE_CURVE('',#2230,#2231,#1408,.T.);
#2699=EDGE_CURVE('',#2225,#2230,#1409,.T.);
#2700=EDGE_CURVE('',#2226,#2231,#1410,.T.);
#2701=EDGE_CURVE('',#2223,#2232,#1411,.T.);
#2702=EDGE_CURVE('',#2232,#2232,#1944,.T.);
#2703=EDGE_CURVE('',#2233,#2234,#1412,.T.);
#2704=EDGE_CURVE('',#2235,#2233,#1413,.T.);
#2705=EDGE_CURVE('',#2236,#2235,#1414,.T.);
#2706=EDGE_CURVE('',#2236,#2234,#1415,.T.);
#2707=EDGE_CURVE('',#2234,#2237,#1416,.T.);
#2708=EDGE_CURVE('',#2238,#2236,#1417,.T.);
#2709=EDGE_CURVE('',#2238,#2237,#1418,.T.);
#2710=EDGE_CURVE('',#2237,#2239,#1419,.T.);
#2711=EDGE_CURVE('',#2240,#2238,#1420,.T.);
#2712=EDGE_CURVE('',#2240,#2239,#1421,.T.);
#2713=EDGE_CURVE('',#2239,#2233,#1422,.T.);
#2714=EDGE_CURVE('',#2235,#2240,#1423,.T.);
#2715=EDGE_CURVE('',#2241,#2242,#1424,.T.);
#2716=EDGE_CURVE('',#2242,#2243,#1425,.T.);
#2717=EDGE_CURVE('',#2244,#2243,#1426,.T.);
#2718=EDGE_CURVE('',#2241,#2244,#1427,.T.);
#2719=EDGE_CURVE('',#2245,#2241,#1428,.T.);
#2720=EDGE_CURVE('',#2246,#2244,#1429,.T.);
#2721=EDGE_CURVE('',#2245,#2246,#1430,.T.);
#2722=EDGE_CURVE('',#2247,#2245,#1431,.T.);
#2723=EDGE_CURVE('',#2248,#2246,#1432,.T.);
#2724=EDGE_CURVE('',#2247,#2248,#1433,.T.);
#2725=EDGE_CURVE('',#2242,#2247,#1434,.T.);
#2726=EDGE_CURVE('',#2243,#2248,#1435,.T.);
#2727=EDGE_CURVE('',#2249,#2249,#1945,.T.);
#2728=EDGE_CURVE('',#2249,#2250,#1436,.T.);
#2729=EDGE_CURVE('',#2250,#2250,#1946,.T.);
#2730=EDGE_CURVE('',#2251,#2251,#1947,.T.);
#2731=EDGE_CURVE('',#2251,#2252,#1437,.T.);
#2732=EDGE_CURVE('',#2252,#2252,#1948,.T.);
#2733=EDGE_CURVE('',#2253,#2254,#1438,.T.);
#2734=EDGE_CURVE('',#2254,#2255,#1439,.T.);
#2735=EDGE_CURVE('',#2256,#2255,#1440,.T.);
#2736=EDGE_CURVE('',#2253,#2256,#1441,.T.);
#2737=EDGE_CURVE('',#2257,#2253,#1442,.T.);
#2738=EDGE_CURVE('',#2258,#2256,#1443,.T.);
#2739=EDGE_CURVE('',#2257,#2258,#1444,.T.);
#2740=EDGE_CURVE('',#2259,#2257,#1445,.T.);
#2741=EDGE_CURVE('',#2260,#2258,#1446,.T.);
#2742=EDGE_CURVE('',#2259,#2260,#1447,.T.);
#2743=EDGE_CURVE('',#2254,#2259,#1448,.T.);
#2744=EDGE_CURVE('',#2255,#2260,#1449,.T.);
#2745=EDGE_CURVE('',#2261,#2262,#1450,.T.);
#2746=EDGE_CURVE('',#2262,#2263,#1451,.T.);
#2747=EDGE_CURVE('',#2263,#2264,#1452,.T.);
#2748=EDGE_CURVE('',#2261,#2264,#1453,.T.);
#2749=EDGE_CURVE('',#2262,#2265,#1454,.T.);
#2750=EDGE_CURVE('',#2265,#2266,#1455,.T.);
#2751=EDGE_CURVE('',#2266,#2263,#1456,.T.);
#2752=EDGE_CURVE('',#2265,#2267,#1457,.T.);
#2753=EDGE_CURVE('',#2267,#2268,#1458,.T.);
#2754=EDGE_CURVE('',#2268,#2266,#1459,.T.);
#2755=EDGE_CURVE('',#2267,#2269,#1460,.T.);
#2756=EDGE_CURVE('',#2269,#2270,#1461,.T.);
#2757=EDGE_CURVE('',#2270,#2268,#1462,.T.);
#2758=EDGE_CURVE('',#2269,#2271,#1463,.T.);
#2759=EDGE_CURVE('',#2271,#2272,#1464,.T.);
#2760=EDGE_CURVE('',#2272,#2270,#1465,.T.);
#2761=EDGE_CURVE('',#2271,#2261,#1466,.T.);
#2762=EDGE_CURVE('',#2264,#2272,#1467,.T.);
#2763=EDGE_CURVE('',#2273,#2273,#1949,.T.);
#2764=EDGE_CURVE('',#2274,#2274,#1950,.T.);
#2765=EDGE_CURVE('',#2275,#2275,#1951,.T.);
#2766=EDGE_CURVE('',#2275,#2274,#1468,.T.);
#2767=EDGE_CURVE('',#2276,#2276,#1952,.T.);
#2768=EDGE_CURVE('',#2276,#2275,#1469,.T.);
#2769=EDGE_CURVE('',#2277,#2277,#1953,.T.);
#2770=EDGE_CURVE('',#2277,#2276,#1470,.T.);
#2771=EDGE_CURVE('',#2278,#2278,#1954,.T.);
#2772=EDGE_CURVE('',#2279,#2279,#1955,.F.);
#2773=EDGE_CURVE('',#2279,#2278,#1471,.T.);
#2774=EDGE_CURVE('',#2273,#2279,#1472,.T.);
#2775=ORIENTED_EDGE('',*,*,#2280,.F.);
#2776=ORIENTED_EDGE('',*,*,#2281,.T.);
#2777=ORIENTED_EDGE('',*,*,#2282,.F.);
#2778=ORIENTED_EDGE('',*,*,#2281,.F.);
#2779=ORIENTED_EDGE('',*,*,#2280,.T.);
#2780=ORIENTED_EDGE('',*,*,#2283,.F.);
#2781=ORIENTED_EDGE('',*,*,#2284,.T.);
#2782=ORIENTED_EDGE('',*,*,#2285,.F.);
#2783=ORIENTED_EDGE('',*,*,#2284,.F.);
#2784=ORIENTED_EDGE('',*,*,#2283,.T.);
#2785=ORIENTED_EDGE('',*,*,#2286,.F.);
#2786=ORIENTED_EDGE('',*,*,#2287,.T.);
#2787=ORIENTED_EDGE('',*,*,#2288,.F.);
#2788=ORIENTED_EDGE('',*,*,#2287,.F.);
#2789=ORIENTED_EDGE('',*,*,#2289,.F.);
#2790=ORIENTED_EDGE('',*,*,#2290,.T.);
#2791=ORIENTED_EDGE('',*,*,#2291,.F.);
#2792=ORIENTED_EDGE('',*,*,#2290,.F.);
#2793=ORIENTED_EDGE('',*,*,#2292,.F.);
#2794=ORIENTED_EDGE('',*,*,#2293,.T.);
#2795=ORIENTED_EDGE('',*,*,#2294,.F.);
#2796=ORIENTED_EDGE('',*,*,#2293,.F.);
#2797=ORIENTED_EDGE('',*,*,#2295,.F.);
#2798=ORIENTED_EDGE('',*,*,#2296,.T.);
#2799=ORIENTED_EDGE('',*,*,#2297,.F.);
#2800=ORIENTED_EDGE('',*,*,#2296,.F.);
#2801=ORIENTED_EDGE('',*,*,#2298,.F.);
#2802=ORIENTED_EDGE('',*,*,#2299,.F.);
#2803=ORIENTED_EDGE('',*,*,#2300,.F.);
#2804=ORIENTED_EDGE('',*,*,#2301,.F.);
#2805=ORIENTED_EDGE('',*,*,#2302,.F.);
#2806=ORIENTED_EDGE('',*,*,#2303,.F.);
#2807=ORIENTED_EDGE('',*,*,#2304,.F.);
#2808=ORIENTED_EDGE('',*,*,#2299,.T.);
#2809=ORIENTED_EDGE('',*,*,#2301,.T.);
#2810=ORIENTED_EDGE('',*,*,#2305,.T.);
#2811=ORIENTED_EDGE('',*,*,#2306,.T.);
#2812=ORIENTED_EDGE('',*,*,#2307,.T.);
#2813=ORIENTED_EDGE('',*,*,#2308,.T.);
#2814=ORIENTED_EDGE('',*,*,#2309,.T.);
#2815=ORIENTED_EDGE('',*,*,#2282,.T.);
#2816=ORIENTED_EDGE('',*,*,#2285,.T.);
#2817=ORIENTED_EDGE('',*,*,#2310,.F.);
#2818=ORIENTED_EDGE('',*,*,#2311,.T.);
#2819=ORIENTED_EDGE('',*,*,#2312,.F.);
#2820=ORIENTED_EDGE('',*,*,#2311,.F.);
#2821=ORIENTED_EDGE('',*,*,#2313,.F.);
#2822=ORIENTED_EDGE('',*,*,#2314,.T.);
#2823=ORIENTED_EDGE('',*,*,#2315,.T.);
#2824=ORIENTED_EDGE('',*,*,#2314,.F.);
#2825=ORIENTED_EDGE('',*,*,#2315,.F.);
#2826=ORIENTED_EDGE('',*,*,#2316,.F.);
#2827=ORIENTED_EDGE('',*,*,#2313,.T.);
#2828=ORIENTED_EDGE('',*,*,#2312,.T.);
#2829=ORIENTED_EDGE('',*,*,#2303,.T.);
#2830=ORIENTED_EDGE('',*,*,#2317,.F.);
#2831=ORIENTED_EDGE('',*,*,#2316,.T.);
#2832=ORIENTED_EDGE('',*,*,#2298,.T.);
#2833=ORIENTED_EDGE('',*,*,#2309,.F.);
#2834=ORIENTED_EDGE('',*,*,#2318,.F.);
#2835=ORIENTED_EDGE('',*,*,#2319,.T.);
#2836=ORIENTED_EDGE('',*,*,#2320,.T.);
#2837=ORIENTED_EDGE('',*,*,#2305,.F.);
#2838=ORIENTED_EDGE('',*,*,#2300,.T.);
#2839=ORIENTED_EDGE('',*,*,#2304,.T.);
#2840=ORIENTED_EDGE('',*,*,#2317,.T.);
#2841=ORIENTED_EDGE('',*,*,#2302,.T.);
#2842=ORIENTED_EDGE('',*,*,#2288,.T.);
#2843=ORIENTED_EDGE('',*,*,#2291,.T.);
#2844=ORIENTED_EDGE('',*,*,#2294,.T.);
#2845=ORIENTED_EDGE('',*,*,#2297,.T.);
#2846=ORIENTED_EDGE('',*,*,#2321,.T.);
#2847=ORIENTED_EDGE('',*,*,#2318,.T.);
#2848=ORIENTED_EDGE('',*,*,#2308,.F.);
#2849=ORIENTED_EDGE('',*,*,#2322,.F.);
#2850=ORIENTED_EDGE('',*,*,#2323,.T.);
#2851=ORIENTED_EDGE('',*,*,#2322,.T.);
#2852=ORIENTED_EDGE('',*,*,#2307,.F.);
#2853=ORIENTED_EDGE('',*,*,#2324,.F.);
#2854=ORIENTED_EDGE('',*,*,#2310,.T.);
#2855=ORIENTED_EDGE('',*,*,#2295,.T.);
#2856=ORIENTED_EDGE('',*,*,#2292,.T.);
#2857=ORIENTED_EDGE('',*,*,#2289,.T.);
#2858=ORIENTED_EDGE('',*,*,#2286,.T.);
#2859=ORIENTED_EDGE('',*,*,#2325,.T.);
#2860=ORIENTED_EDGE('',*,*,#2324,.T.);
#2861=ORIENTED_EDGE('',*,*,#2306,.F.);
#2862=ORIENTED_EDGE('',*,*,#2320,.F.);
#2863=ORIENTED_EDGE('',*,*,#2325,.F.);
#2864=ORIENTED_EDGE('',*,*,#2319,.F.);
#2865=ORIENTED_EDGE('',*,*,#2321,.F.);
#2866=ORIENTED_EDGE('',*,*,#2323,.F.);
#2867=ORIENTED_EDGE('',*,*,#2326,.F.);
#2868=ORIENTED_EDGE('',*,*,#2327,.F.);
#2869=ORIENTED_EDGE('',*,*,#2327,.T.);
#2870=ORIENTED_EDGE('',*,*,#2328,.T.);
#2871=ORIENTED_EDGE('',*,*,#2329,.T.);
#2872=ORIENTED_EDGE('',*,*,#2328,.F.);
#2873=ORIENTED_EDGE('',*,*,#2330,.F.);
#2874=ORIENTED_EDGE('',*,*,#2331,.T.);
#2875=ORIENTED_EDGE('',*,*,#2332,.T.);
#2876=ORIENTED_EDGE('',*,*,#2331,.F.);
#2877=ORIENTED_EDGE('',*,*,#2330,.T.);
#2878=ORIENTED_EDGE('',*,*,#2326,.T.);
#2879=ORIENTED_EDGE('',*,*,#2332,.F.);
#2880=ORIENTED_EDGE('',*,*,#2329,.F.);
#2881=ORIENTED_EDGE('',*,*,#2333,.F.);
#2882=ORIENTED_EDGE('',*,*,#2334,.T.);
#2883=ORIENTED_EDGE('',*,*,#2335,.F.);
#2884=ORIENTED_EDGE('',*,*,#2334,.F.);
#2885=ORIENTED_EDGE('',*,*,#2333,.T.);
#2886=ORIENTED_EDGE('',*,*,#2336,.F.);
#2887=ORIENTED_EDGE('',*,*,#2337,.T.);
#2888=ORIENTED_EDGE('',*,*,#2338,.F.);
#2889=ORIENTED_EDGE('',*,*,#2337,.F.);
#2890=ORIENTED_EDGE('',*,*,#2336,.T.);
#2891=ORIENTED_EDGE('',*,*,#2339,.F.);
#2892=ORIENTED_EDGE('',*,*,#2340,.T.);
#2893=ORIENTED_EDGE('',*,*,#2341,.F.);
#2894=ORIENTED_EDGE('',*,*,#2340,.F.);
#2895=ORIENTED_EDGE('',*,*,#2342,.F.);
#2896=ORIENTED_EDGE('',*,*,#2343,.T.);
#2897=ORIENTED_EDGE('',*,*,#2344,.F.);
#2898=ORIENTED_EDGE('',*,*,#2343,.F.);
#2899=ORIENTED_EDGE('',*,*,#2345,.F.);
#2900=ORIENTED_EDGE('',*,*,#2346,.T.);
#2901=ORIENTED_EDGE('',*,*,#2347,.F.);
#2902=ORIENTED_EDGE('',*,*,#2346,.F.);
#2903=ORIENTED_EDGE('',*,*,#2348,.F.);
#2904=ORIENTED_EDGE('',*,*,#2349,.T.);
#2905=ORIENTED_EDGE('',*,*,#2350,.F.);
#2906=ORIENTED_EDGE('',*,*,#2349,.F.);
#2907=ORIENTED_EDGE('',*,*,#2351,.F.);
#2908=ORIENTED_EDGE('',*,*,#2352,.F.);
#2909=ORIENTED_EDGE('',*,*,#2353,.F.);
#2910=ORIENTED_EDGE('',*,*,#2354,.F.);
#2911=ORIENTED_EDGE('',*,*,#2355,.F.);
#2912=ORIENTED_EDGE('',*,*,#2356,.F.);
#2913=ORIENTED_EDGE('',*,*,#2357,.F.);
#2914=ORIENTED_EDGE('',*,*,#2352,.T.);
#2915=ORIENTED_EDGE('',*,*,#2354,.T.);
#2916=ORIENTED_EDGE('',*,*,#2358,.T.);
#2917=ORIENTED_EDGE('',*,*,#2359,.T.);
#2918=ORIENTED_EDGE('',*,*,#2360,.T.);
#2919=ORIENTED_EDGE('',*,*,#2361,.T.);
#2920=ORIENTED_EDGE('',*,*,#2362,.T.);
#2921=ORIENTED_EDGE('',*,*,#2335,.T.);
#2922=ORIENTED_EDGE('',*,*,#2338,.T.);
#2923=ORIENTED_EDGE('',*,*,#2363,.F.);
#2924=ORIENTED_EDGE('',*,*,#2364,.T.);
#2925=ORIENTED_EDGE('',*,*,#2365,.F.);
#2926=ORIENTED_EDGE('',*,*,#2364,.F.);
#2927=ORIENTED_EDGE('',*,*,#2366,.F.);
#2928=ORIENTED_EDGE('',*,*,#2367,.T.);
#2929=ORIENTED_EDGE('',*,*,#2368,.T.);
#2930=ORIENTED_EDGE('',*,*,#2367,.F.);
#2931=ORIENTED_EDGE('',*,*,#2368,.F.);
#2932=ORIENTED_EDGE('',*,*,#2363,.T.);
#2933=ORIENTED_EDGE('',*,*,#2366,.T.);
#2934=ORIENTED_EDGE('',*,*,#2369,.F.);
#2935=ORIENTED_EDGE('',*,*,#2356,.T.);
#2936=ORIENTED_EDGE('',*,*,#2370,.F.);
#2937=ORIENTED_EDGE('',*,*,#2369,.T.);
#2938=ORIENTED_EDGE('',*,*,#2371,.T.);
#2939=ORIENTED_EDGE('',*,*,#2372,.T.);
#2940=ORIENTED_EDGE('',*,*,#2360,.F.);
#2941=ORIENTED_EDGE('',*,*,#2373,.F.);
#2942=ORIENTED_EDGE('',*,*,#2365,.T.);
#2943=ORIENTED_EDGE('',*,*,#2350,.T.);
#2944=ORIENTED_EDGE('',*,*,#2347,.T.);
#2945=ORIENTED_EDGE('',*,*,#2344,.T.);
#2946=ORIENTED_EDGE('',*,*,#2341,.T.);
#2947=ORIENTED_EDGE('',*,*,#2374,.T.);
#2948=ORIENTED_EDGE('',*,*,#2373,.T.);
#2949=ORIENTED_EDGE('',*,*,#2359,.F.);
#2950=ORIENTED_EDGE('',*,*,#2375,.F.);
#2951=ORIENTED_EDGE('',*,*,#2351,.T.);
#2952=ORIENTED_EDGE('',*,*,#2362,.F.);
#2953=ORIENTED_EDGE('',*,*,#2376,.F.);
#2954=ORIENTED_EDGE('',*,*,#2377,.T.);
#2955=ORIENTED_EDGE('',*,*,#2375,.T.);
#2956=ORIENTED_EDGE('',*,*,#2358,.F.);
#2957=ORIENTED_EDGE('',*,*,#2353,.T.);
#2958=ORIENTED_EDGE('',*,*,#2357,.T.);
#2959=ORIENTED_EDGE('',*,*,#2370,.T.);
#2960=ORIENTED_EDGE('',*,*,#2355,.T.);
#2961=ORIENTED_EDGE('',*,*,#2339,.T.);
#2962=ORIENTED_EDGE('',*,*,#2342,.T.);
#2963=ORIENTED_EDGE('',*,*,#2345,.T.);
#2964=ORIENTED_EDGE('',*,*,#2348,.T.);
#2965=ORIENTED_EDGE('',*,*,#2378,.T.);
#2966=ORIENTED_EDGE('',*,*,#2376,.T.);
#2967=ORIENTED_EDGE('',*,*,#2361,.F.);
#2968=ORIENTED_EDGE('',*,*,#2372,.F.);
#2969=ORIENTED_EDGE('',*,*,#2378,.F.);
#2970=ORIENTED_EDGE('',*,*,#2371,.F.);
#2971=ORIENTED_EDGE('',*,*,#2374,.F.);
#2972=ORIENTED_EDGE('',*,*,#2377,.F.);
#2973=ORIENTED_EDGE('',*,*,#2379,.F.);
#2974=ORIENTED_EDGE('',*,*,#2380,.F.);
#2975=ORIENTED_EDGE('',*,*,#2381,.F.);
#2976=ORIENTED_EDGE('',*,*,#2382,.T.);
#2977=ORIENTED_EDGE('',*,*,#2380,.T.);
#2978=ORIENTED_EDGE('',*,*,#2382,.F.);
#2979=ORIENTED_EDGE('',*,*,#2383,.F.);
#2980=ORIENTED_EDGE('',*,*,#2384,.T.);
#2981=ORIENTED_EDGE('',*,*,#2385,.T.);
#2982=ORIENTED_EDGE('',*,*,#2384,.F.);
#2983=ORIENTED_EDGE('',*,*,#2383,.T.);
#2984=ORIENTED_EDGE('',*,*,#2381,.T.);
#2985=ORIENTED_EDGE('',*,*,#2385,.F.);
#2986=ORIENTED_EDGE('',*,*,#2379,.T.);
#2987=ORIENTED_EDGE('',*,*,#2386,.F.);
#2988=ORIENTED_EDGE('',*,*,#2387,.T.);
#2989=ORIENTED_EDGE('',*,*,#2388,.F.);
#2990=ORIENTED_EDGE('',*,*,#2387,.F.);
#2991=ORIENTED_EDGE('',*,*,#2389,.F.);
#2992=ORIENTED_EDGE('',*,*,#2390,.T.);
#2993=ORIENTED_EDGE('',*,*,#2391,.F.);
#2994=ORIENTED_EDGE('',*,*,#2390,.F.);
#2995=ORIENTED_EDGE('',*,*,#2392,.F.);
#2996=ORIENTED_EDGE('',*,*,#2393,.T.);
#2997=ORIENTED_EDGE('',*,*,#2394,.F.);
#2998=ORIENTED_EDGE('',*,*,#2393,.F.);
#2999=ORIENTED_EDGE('',*,*,#2395,.F.);
#3000=ORIENTED_EDGE('',*,*,#2396,.T.);
#3001=ORIENTED_EDGE('',*,*,#2397,.F.);
#3002=ORIENTED_EDGE('',*,*,#2396,.F.);
#3003=ORIENTED_EDGE('',*,*,#2398,.F.);
#3004=ORIENTED_EDGE('',*,*,#2399,.T.);
#3005=ORIENTED_EDGE('',*,*,#2400,.F.);
#3006=ORIENTED_EDGE('',*,*,#2401,.F.);
#3007=ORIENTED_EDGE('',*,*,#2402,.F.);
#3008=ORIENTED_EDGE('',*,*,#2403,.T.);
#3009=ORIENTED_EDGE('',*,*,#2404,.F.);
#3010=ORIENTED_EDGE('',*,*,#2405,.F.);
#3011=ORIENTED_EDGE('',*,*,#2406,.F.);
#3012=ORIENTED_EDGE('',*,*,#2407,.F.);
#3013=ORIENTED_EDGE('',*,*,#2408,.F.);
#3014=ORIENTED_EDGE('',*,*,#2399,.F.);
#3015=ORIENTED_EDGE('',*,*,#2409,.F.);
#3016=ORIENTED_EDGE('',*,*,#2410,.F.);
#3017=ORIENTED_EDGE('',*,*,#2411,.F.);
#3018=ORIENTED_EDGE('',*,*,#2403,.F.);
#3019=ORIENTED_EDGE('',*,*,#2400,.T.);
#3020=ORIENTED_EDGE('',*,*,#2408,.T.);
#3021=ORIENTED_EDGE('',*,*,#2412,.T.);
#3022=ORIENTED_EDGE('',*,*,#2404,.T.);
#3023=ORIENTED_EDGE('',*,*,#2411,.T.);
#3024=ORIENTED_EDGE('',*,*,#2413,.T.);
#3025=ORIENTED_EDGE('',*,*,#2414,.T.);
#3026=ORIENTED_EDGE('',*,*,#2415,.T.);
#3027=ORIENTED_EDGE('',*,*,#2416,.T.);
#3028=ORIENTED_EDGE('',*,*,#2417,.T.);
#3029=ORIENTED_EDGE('',*,*,#2388,.T.);
#3030=ORIENTED_EDGE('',*,*,#2391,.T.);
#3031=ORIENTED_EDGE('',*,*,#2394,.T.);
#3032=ORIENTED_EDGE('',*,*,#2397,.T.);
#3033=ORIENTED_EDGE('',*,*,#2410,.T.);
#3034=ORIENTED_EDGE('',*,*,#2418,.F.);
#3035=ORIENTED_EDGE('',*,*,#2419,.T.);
#3036=ORIENTED_EDGE('',*,*,#2413,.F.);
#3037=ORIENTED_EDGE('',*,*,#2401,.T.);
#3038=ORIENTED_EDGE('',*,*,#2417,.F.);
#3039=ORIENTED_EDGE('',*,*,#2420,.F.);
#3040=ORIENTED_EDGE('',*,*,#2421,.F.);
#3041=ORIENTED_EDGE('',*,*,#2407,.T.);
#3042=ORIENTED_EDGE('',*,*,#2422,.F.);
#3043=ORIENTED_EDGE('',*,*,#2405,.T.);
#3044=ORIENTED_EDGE('',*,*,#2412,.F.);
#3045=ORIENTED_EDGE('',*,*,#2423,.F.);
#3046=ORIENTED_EDGE('',*,*,#2420,.T.);
#3047=ORIENTED_EDGE('',*,*,#2416,.F.);
#3048=ORIENTED_EDGE('',*,*,#2424,.F.);
#3049=ORIENTED_EDGE('',*,*,#2425,.F.);
#3050=ORIENTED_EDGE('',*,*,#2424,.T.);
#3051=ORIENTED_EDGE('',*,*,#2415,.F.);
#3052=ORIENTED_EDGE('',*,*,#2426,.F.);
#3053=ORIENTED_EDGE('',*,*,#2427,.F.);
#3054=ORIENTED_EDGE('',*,*,#2426,.T.);
#3055=ORIENTED_EDGE('',*,*,#2414,.F.);
#3056=ORIENTED_EDGE('',*,*,#2419,.F.);
#3057=ORIENTED_EDGE('',*,*,#2398,.T.);
#3058=ORIENTED_EDGE('',*,*,#2421,.T.);
#3059=ORIENTED_EDGE('',*,*,#2423,.T.);
#3060=ORIENTED_EDGE('',*,*,#2425,.T.);
#3061=ORIENTED_EDGE('',*,*,#2427,.T.);
#3062=ORIENTED_EDGE('',*,*,#2418,.T.);
#3063=ORIENTED_EDGE('',*,*,#2409,.T.);
#3064=ORIENTED_EDGE('',*,*,#2402,.T.);
#3065=ORIENTED_EDGE('',*,*,#2422,.T.);
#3066=ORIENTED_EDGE('',*,*,#2406,.T.);
#3067=ORIENTED_EDGE('',*,*,#2386,.T.);
#3068=ORIENTED_EDGE('',*,*,#2389,.T.);
#3069=ORIENTED_EDGE('',*,*,#2392,.T.);
#3070=ORIENTED_EDGE('',*,*,#2395,.T.);
#3071=ORIENTED_EDGE('',*,*,#2428,.F.);
#3072=ORIENTED_EDGE('',*,*,#2429,.T.);
#3073=ORIENTED_EDGE('',*,*,#2430,.F.);
#3074=ORIENTED_EDGE('',*,*,#2431,.T.);
#3075=ORIENTED_EDGE('',*,*,#2428,.T.);
#3076=ORIENTED_EDGE('',*,*,#2431,.F.);
#3077=ORIENTED_EDGE('',*,*,#2430,.T.);
#3078=ORIENTED_EDGE('',*,*,#2432,.T.);
#3079=ORIENTED_EDGE('',*,*,#2432,.F.);
#3080=ORIENTED_EDGE('',*,*,#2433,.T.);
#3081=ORIENTED_EDGE('',*,*,#2434,.T.);
#3082=ORIENTED_EDGE('',*,*,#2433,.F.);
#3083=ORIENTED_EDGE('',*,*,#2429,.F.);
#3084=ORIENTED_EDGE('',*,*,#2435,.T.);
#3085=ORIENTED_EDGE('',*,*,#2436,.T.);
#3086=ORIENTED_EDGE('',*,*,#2435,.F.);
#3087=ORIENTED_EDGE('',*,*,#2436,.F.);
#3088=ORIENTED_EDGE('',*,*,#2434,.F.);
#3089=ORIENTED_EDGE('',*,*,#2437,.F.);
#3090=ORIENTED_EDGE('',*,*,#2438,.T.);
#3091=ORIENTED_EDGE('',*,*,#2437,.T.);
#3092=ORIENTED_EDGE('',*,*,#2438,.F.);
#3093=ORIENTED_EDGE('',*,*,#2439,.F.);
#3094=ORIENTED_EDGE('',*,*,#2440,.T.);
#3095=ORIENTED_EDGE('',*,*,#2441,.T.);
#3096=ORIENTED_EDGE('',*,*,#2440,.F.);
#3097=ORIENTED_EDGE('',*,*,#2441,.F.);
#3098=ORIENTED_EDGE('',*,*,#2442,.F.);
#3099=ORIENTED_EDGE('',*,*,#2443,.F.);
#3100=ORIENTED_EDGE('',*,*,#2444,.T.);
#3101=ORIENTED_EDGE('',*,*,#2442,.T.);
#3102=ORIENTED_EDGE('',*,*,#2444,.F.);
#3103=ORIENTED_EDGE('',*,*,#2445,.F.);
#3104=ORIENTED_EDGE('',*,*,#2446,.T.);
#3105=ORIENTED_EDGE('',*,*,#2447,.T.);
#3106=ORIENTED_EDGE('',*,*,#2446,.F.);
#3107=ORIENTED_EDGE('',*,*,#2445,.T.);
#3108=ORIENTED_EDGE('',*,*,#2443,.T.);
#3109=ORIENTED_EDGE('',*,*,#2447,.F.);
#3110=ORIENTED_EDGE('',*,*,#2439,.T.);
#3111=ORIENTED_EDGE('',*,*,#2448,.F.);
#3112=ORIENTED_EDGE('',*,*,#2449,.T.);
#3113=ORIENTED_EDGE('',*,*,#2450,.F.);
#3114=ORIENTED_EDGE('',*,*,#2449,.F.);
#3115=ORIENTED_EDGE('',*,*,#2448,.T.);
#3116=ORIENTED_EDGE('',*,*,#2451,.F.);
#3117=ORIENTED_EDGE('',*,*,#2452,.T.);
#3118=ORIENTED_EDGE('',*,*,#2453,.F.);
#3119=ORIENTED_EDGE('',*,*,#2452,.F.);
#3120=ORIENTED_EDGE('',*,*,#2451,.T.);
#3121=ORIENTED_EDGE('',*,*,#2454,.F.);
#3122=ORIENTED_EDGE('',*,*,#2455,.T.);
#3123=ORIENTED_EDGE('',*,*,#2456,.F.);
#3124=ORIENTED_EDGE('',*,*,#2455,.F.);
#3125=ORIENTED_EDGE('',*,*,#2457,.F.);
#3126=ORIENTED_EDGE('',*,*,#2458,.T.);
#3127=ORIENTED_EDGE('',*,*,#2459,.F.);
#3128=ORIENTED_EDGE('',*,*,#2458,.F.);
#3129=ORIENTED_EDGE('',*,*,#2460,.F.);
#3130=ORIENTED_EDGE('',*,*,#2461,.T.);
#3131=ORIENTED_EDGE('',*,*,#2462,.F.);
#3132=ORIENTED_EDGE('',*,*,#2461,.F.);
#3133=ORIENTED_EDGE('',*,*,#2463,.F.);
#3134=ORIENTED_EDGE('',*,*,#2464,.T.);
#3135=ORIENTED_EDGE('',*,*,#2465,.F.);
#3136=ORIENTED_EDGE('',*,*,#2464,.F.);
#3137=ORIENTED_EDGE('',*,*,#2466,.F.);
#3138=ORIENTED_EDGE('',*,*,#2467,.T.);
#3139=ORIENTED_EDGE('',*,*,#2468,.F.);
#3140=ORIENTED_EDGE('',*,*,#2467,.F.);
#3141=ORIENTED_EDGE('',*,*,#2469,.T.);
#3142=ORIENTED_EDGE('',*,*,#2470,.T.);
#3143=ORIENTED_EDGE('',*,*,#2471,.F.);
#3144=ORIENTED_EDGE('',*,*,#2472,.F.);
#3145=ORIENTED_EDGE('',*,*,#2473,.T.);
#3146=ORIENTED_EDGE('',*,*,#2472,.T.);
#3147=ORIENTED_EDGE('',*,*,#2474,.F.);
#3148=ORIENTED_EDGE('',*,*,#2475,.F.);
#3149=ORIENTED_EDGE('',*,*,#2476,.T.);
#3150=ORIENTED_EDGE('',*,*,#2475,.T.);
#3151=ORIENTED_EDGE('',*,*,#2477,.F.);
#3152=ORIENTED_EDGE('',*,*,#2478,.F.);
#3153=ORIENTED_EDGE('',*,*,#2479,.T.);
#3154=ORIENTED_EDGE('',*,*,#2478,.T.);
#3155=ORIENTED_EDGE('',*,*,#2480,.F.);
#3156=ORIENTED_EDGE('',*,*,#2470,.F.);
#3157=ORIENTED_EDGE('',*,*,#2480,.T.);
#3158=ORIENTED_EDGE('',*,*,#2477,.T.);
#3159=ORIENTED_EDGE('',*,*,#2474,.T.);
#3160=ORIENTED_EDGE('',*,*,#2471,.T.);
#3161=ORIENTED_EDGE('',*,*,#2450,.T.);
#3162=ORIENTED_EDGE('',*,*,#2453,.T.);
#3163=ORIENTED_EDGE('',*,*,#2468,.T.);
#3164=ORIENTED_EDGE('',*,*,#2465,.T.);
#3165=ORIENTED_EDGE('',*,*,#2462,.T.);
#3166=ORIENTED_EDGE('',*,*,#2459,.T.);
#3167=ORIENTED_EDGE('',*,*,#2456,.T.);
#3168=ORIENTED_EDGE('',*,*,#2479,.F.);
#3169=ORIENTED_EDGE('',*,*,#2469,.F.);
#3170=ORIENTED_EDGE('',*,*,#2473,.F.);
#3171=ORIENTED_EDGE('',*,*,#2476,.F.);
#3172=ORIENTED_EDGE('',*,*,#2466,.T.);
#3173=ORIENTED_EDGE('',*,*,#2463,.T.);
#3174=ORIENTED_EDGE('',*,*,#2460,.T.);
#3175=ORIENTED_EDGE('',*,*,#2457,.T.);
#3176=ORIENTED_EDGE('',*,*,#2454,.T.);
#3177=ORIENTED_EDGE('',*,*,#2481,.F.);
#3178=ORIENTED_EDGE('',*,*,#2482,.T.);
#3179=ORIENTED_EDGE('',*,*,#2483,.T.);
#3180=ORIENTED_EDGE('',*,*,#2482,.F.);
#3181=ORIENTED_EDGE('',*,*,#2484,.F.);
#3182=ORIENTED_EDGE('',*,*,#2485,.T.);
#3183=ORIENTED_EDGE('',*,*,#2486,.T.);
#3184=ORIENTED_EDGE('',*,*,#2485,.F.);
#3185=ORIENTED_EDGE('',*,*,#2484,.T.);
#3186=ORIENTED_EDGE('',*,*,#2481,.T.);
#3187=ORIENTED_EDGE('',*,*,#2486,.F.);
#3188=ORIENTED_EDGE('',*,*,#2483,.F.);
#3189=ORIENTED_EDGE('',*,*,#2487,.F.);
#3190=ORIENTED_EDGE('',*,*,#2488,.T.);
#3191=ORIENTED_EDGE('',*,*,#2489,.T.);
#3192=ORIENTED_EDGE('',*,*,#2488,.F.);
#3193=ORIENTED_EDGE('',*,*,#2490,.F.);
#3194=ORIENTED_EDGE('',*,*,#2491,.T.);
#3195=ORIENTED_EDGE('',*,*,#2492,.T.);
#3196=ORIENTED_EDGE('',*,*,#2491,.F.);
#3197=ORIENTED_EDGE('',*,*,#2490,.T.);
#3198=ORIENTED_EDGE('',*,*,#2487,.T.);
#3199=ORIENTED_EDGE('',*,*,#2492,.F.);
#3200=ORIENTED_EDGE('',*,*,#2489,.F.);
#3201=ORIENTED_EDGE('',*,*,#2493,.F.);
#3202=ORIENTED_EDGE('',*,*,#2494,.T.);
#3203=ORIENTED_EDGE('',*,*,#2495,.T.);
#3204=ORIENTED_EDGE('',*,*,#2494,.F.);
#3205=ORIENTED_EDGE('',*,*,#2496,.F.);
#3206=ORIENTED_EDGE('',*,*,#2497,.T.);
#3207=ORIENTED_EDGE('',*,*,#2498,.T.);
#3208=ORIENTED_EDGE('',*,*,#2497,.F.);
#3209=ORIENTED_EDGE('',*,*,#2496,.T.);
#3210=ORIENTED_EDGE('',*,*,#2493,.T.);
#3211=ORIENTED_EDGE('',*,*,#2498,.F.);
#3212=ORIENTED_EDGE('',*,*,#2495,.F.);
#3213=ORIENTED_EDGE('',*,*,#2499,.F.);
#3214=ORIENTED_EDGE('',*,*,#2500,.T.);
#3215=ORIENTED_EDGE('',*,*,#2501,.T.);
#3216=ORIENTED_EDGE('',*,*,#2500,.F.);
#3217=ORIENTED_EDGE('',*,*,#2502,.F.);
#3218=ORIENTED_EDGE('',*,*,#2503,.T.);
#3219=ORIENTED_EDGE('',*,*,#2504,.T.);
#3220=ORIENTED_EDGE('',*,*,#2503,.F.);
#3221=ORIENTED_EDGE('',*,*,#2502,.T.);
#3222=ORIENTED_EDGE('',*,*,#2499,.T.);
#3223=ORIENTED_EDGE('',*,*,#2504,.F.);
#3224=ORIENTED_EDGE('',*,*,#2501,.F.);
#3225=ORIENTED_EDGE('',*,*,#2505,.F.);
#3226=ORIENTED_EDGE('',*,*,#2506,.T.);
#3227=ORIENTED_EDGE('',*,*,#2507,.T.);
#3228=ORIENTED_EDGE('',*,*,#2506,.F.);
#3229=ORIENTED_EDGE('',*,*,#2505,.T.);
#3230=ORIENTED_EDGE('',*,*,#2507,.F.);
#3231=ORIENTED_EDGE('',*,*,#2508,.F.);
#3232=ORIENTED_EDGE('',*,*,#2509,.T.);
#3233=ORIENTED_EDGE('',*,*,#2510,.T.);
#3234=ORIENTED_EDGE('',*,*,#2509,.F.);
#3235=ORIENTED_EDGE('',*,*,#2508,.T.);
#3236=ORIENTED_EDGE('',*,*,#2510,.F.);
#3237=ORIENTED_EDGE('',*,*,#2511,.T.);
#3238=ORIENTED_EDGE('',*,*,#2512,.T.);
#3239=ORIENTED_EDGE('',*,*,#2513,.T.);
#3240=ORIENTED_EDGE('',*,*,#2514,.F.);
#3241=ORIENTED_EDGE('',*,*,#2515,.T.);
#3242=ORIENTED_EDGE('',*,*,#2516,.T.);
#3243=ORIENTED_EDGE('',*,*,#2517,.T.);
#3244=ORIENTED_EDGE('',*,*,#2512,.F.);
#3245=ORIENTED_EDGE('',*,*,#2518,.T.);
#3246=ORIENTED_EDGE('',*,*,#2519,.T.);
#3247=ORIENTED_EDGE('',*,*,#2520,.T.);
#3248=ORIENTED_EDGE('',*,*,#2516,.F.);
#3249=ORIENTED_EDGE('',*,*,#2521,.T.);
#3250=ORIENTED_EDGE('',*,*,#2522,.T.);
#3251=ORIENTED_EDGE('',*,*,#2523,.T.);
#3252=ORIENTED_EDGE('',*,*,#2519,.F.);
#3253=ORIENTED_EDGE('',*,*,#2524,.T.);
#3254=ORIENTED_EDGE('',*,*,#2525,.T.);
#3255=ORIENTED_EDGE('',*,*,#2526,.T.);
#3256=ORIENTED_EDGE('',*,*,#2522,.F.);
#3257=ORIENTED_EDGE('',*,*,#2527,.T.);
#3258=ORIENTED_EDGE('',*,*,#2514,.T.);
#3259=ORIENTED_EDGE('',*,*,#2528,.T.);
#3260=ORIENTED_EDGE('',*,*,#2525,.F.);
#3261=ORIENTED_EDGE('',*,*,#2527,.F.);
#3262=ORIENTED_EDGE('',*,*,#2524,.F.);
#3263=ORIENTED_EDGE('',*,*,#2521,.F.);
#3264=ORIENTED_EDGE('',*,*,#2518,.F.);
#3265=ORIENTED_EDGE('',*,*,#2515,.F.);
#3266=ORIENTED_EDGE('',*,*,#2511,.F.);
#3267=ORIENTED_EDGE('',*,*,#2528,.F.);
#3268=ORIENTED_EDGE('',*,*,#2513,.F.);
#3269=ORIENTED_EDGE('',*,*,#2517,.F.);
#3270=ORIENTED_EDGE('',*,*,#2520,.F.);
#3271=ORIENTED_EDGE('',*,*,#2523,.F.);
#3272=ORIENTED_EDGE('',*,*,#2526,.F.);
#3273=ORIENTED_EDGE('',*,*,#2529,.T.);
#3274=ORIENTED_EDGE('',*,*,#2530,.F.);
#3275=ORIENTED_EDGE('',*,*,#2529,.F.);
#3276=ORIENTED_EDGE('',*,*,#2531,.T.);
#3277=ORIENTED_EDGE('',*,*,#2532,.T.);
#3278=ORIENTED_EDGE('',*,*,#2531,.F.);
#3279=ORIENTED_EDGE('',*,*,#2532,.F.);
#3280=ORIENTED_EDGE('',*,*,#2533,.F.);
#3281=ORIENTED_EDGE('',*,*,#2534,.F.);
#3282=ORIENTED_EDGE('',*,*,#2535,.T.);
#3283=ORIENTED_EDGE('',*,*,#2533,.T.);
#3284=ORIENTED_EDGE('',*,*,#2535,.F.);
#3285=ORIENTED_EDGE('',*,*,#2536,.F.);
#3286=ORIENTED_EDGE('',*,*,#2537,.T.);
#3287=ORIENTED_EDGE('',*,*,#2534,.T.);
#3288=ORIENTED_EDGE('',*,*,#2537,.F.);
#3289=ORIENTED_EDGE('',*,*,#2538,.F.);
#3290=ORIENTED_EDGE('',*,*,#2539,.T.);
#3291=ORIENTED_EDGE('',*,*,#2536,.T.);
#3292=ORIENTED_EDGE('',*,*,#2539,.F.);
#3293=ORIENTED_EDGE('',*,*,#2538,.T.);
#3294=ORIENTED_EDGE('',*,*,#2540,.F.);
#3295=ORIENTED_EDGE('',*,*,#2541,.F.);
#3296=ORIENTED_EDGE('',*,*,#2542,.T.);
#3297=ORIENTED_EDGE('',*,*,#2540,.T.);
#3298=ORIENTED_EDGE('',*,*,#2542,.F.);
#3299=ORIENTED_EDGE('',*,*,#2530,.T.);
#3300=ORIENTED_EDGE('',*,*,#2543,.T.);
#3301=ORIENTED_EDGE('',*,*,#2541,.T.);
#3302=ORIENTED_EDGE('',*,*,#2543,.F.);
#3303=ORIENTED_EDGE('',*,*,#2544,.T.);
#3304=ORIENTED_EDGE('',*,*,#2545,.T.);
#3305=ORIENTED_EDGE('',*,*,#2546,.T.);
#3306=ORIENTED_EDGE('',*,*,#2545,.F.);
#3307=ORIENTED_EDGE('',*,*,#2546,.F.);
#3308=ORIENTED_EDGE('',*,*,#2547,.T.);
#3309=ORIENTED_EDGE('',*,*,#2548,.T.);
#3310=ORIENTED_EDGE('',*,*,#2547,.F.);
#3311=ORIENTED_EDGE('',*,*,#2549,.T.);
#3312=ORIENTED_EDGE('',*,*,#2544,.F.);
#3313=ORIENTED_EDGE('',*,*,#2549,.F.);
#3314=ORIENTED_EDGE('',*,*,#2550,.T.);
#3315=ORIENTED_EDGE('',*,*,#2551,.T.);
#3316=ORIENTED_EDGE('',*,*,#2550,.F.);
#3317=ORIENTED_EDGE('',*,*,#2551,.F.);
#3318=ORIENTED_EDGE('',*,*,#2548,.F.);
#3319=ORIENTED_EDGE('',*,*,#2552,.F.);
#3320=ORIENTED_EDGE('',*,*,#2553,.F.);
#3321=ORIENTED_EDGE('',*,*,#2554,.T.);
#3322=ORIENTED_EDGE('',*,*,#2555,.F.);
#3323=ORIENTED_EDGE('',*,*,#2554,.F.);
#3324=ORIENTED_EDGE('',*,*,#2556,.F.);
#3325=ORIENTED_EDGE('',*,*,#2557,.F.);
#3326=ORIENTED_EDGE('',*,*,#2558,.F.);
#3327=ORIENTED_EDGE('',*,*,#2559,.F.);
#3328=ORIENTED_EDGE('',*,*,#2560,.F.);
#3329=ORIENTED_EDGE('',*,*,#2561,.T.);
#3330=ORIENTED_EDGE('',*,*,#2562,.F.);
#3331=ORIENTED_EDGE('',*,*,#2563,.F.);
#3332=ORIENTED_EDGE('',*,*,#2564,.F.);
#3333=ORIENTED_EDGE('',*,*,#2565,.F.);
#3334=ORIENTED_EDGE('',*,*,#2566,.F.);
#3335=ORIENTED_EDGE('',*,*,#2567,.F.);
#3336=ORIENTED_EDGE('',*,*,#2561,.F.);
#3337=ORIENTED_EDGE('',*,*,#2557,.T.);
#3338=ORIENTED_EDGE('',*,*,#2568,.T.);
#3339=ORIENTED_EDGE('',*,*,#2566,.T.);
#3340=ORIENTED_EDGE('',*,*,#2569,.F.);
#3341=ORIENTED_EDGE('',*,*,#2556,.T.);
#3342=ORIENTED_EDGE('',*,*,#2570,.T.);
#3343=ORIENTED_EDGE('',*,*,#2567,.T.);
#3344=ORIENTED_EDGE('',*,*,#2568,.F.);
#3345=ORIENTED_EDGE('',*,*,#2553,.T.);
#3346=ORIENTED_EDGE('',*,*,#2571,.T.);
#3347=ORIENTED_EDGE('',*,*,#2562,.T.);
#3348=ORIENTED_EDGE('',*,*,#2570,.F.);
#3349=ORIENTED_EDGE('',*,*,#2572,.F.);
#3350=ORIENTED_EDGE('',*,*,#2573,.T.);
#3351=ORIENTED_EDGE('',*,*,#2574,.T.);
#3352=ORIENTED_EDGE('',*,*,#2573,.F.);
#3353=ORIENTED_EDGE('',*,*,#2552,.T.);
#3354=ORIENTED_EDGE('',*,*,#2575,.T.);
#3355=ORIENTED_EDGE('',*,*,#2563,.T.);
#3356=ORIENTED_EDGE('',*,*,#2571,.F.);
#3357=ORIENTED_EDGE('',*,*,#2558,.T.);
#3358=ORIENTED_EDGE('',*,*,#2569,.T.);
#3359=ORIENTED_EDGE('',*,*,#2565,.T.);
#3360=ORIENTED_EDGE('',*,*,#2576,.F.);
#3361=ORIENTED_EDGE('',*,*,#2559,.T.);
#3362=ORIENTED_EDGE('',*,*,#2576,.T.);
#3363=ORIENTED_EDGE('',*,*,#2564,.T.);
#3364=ORIENTED_EDGE('',*,*,#2575,.F.);
#3365=ORIENTED_EDGE('',*,*,#2560,.T.);
#3366=ORIENTED_EDGE('',*,*,#2572,.T.);
#3367=ORIENTED_EDGE('',*,*,#2555,.T.);
#3368=ORIENTED_EDGE('',*,*,#2574,.F.);
#3369=ORIENTED_EDGE('',*,*,#2577,.T.);
#3370=ORIENTED_EDGE('',*,*,#2578,.T.);
#3371=ORIENTED_EDGE('',*,*,#2579,.T.);
#3372=ORIENTED_EDGE('',*,*,#2580,.T.);
#3373=ORIENTED_EDGE('',*,*,#2581,.T.);
#3374=ORIENTED_EDGE('',*,*,#2582,.T.);
#3375=ORIENTED_EDGE('',*,*,#2583,.F.);
#3376=ORIENTED_EDGE('',*,*,#2584,.T.);
#3377=ORIENTED_EDGE('',*,*,#2585,.T.);
#3378=ORIENTED_EDGE('',*,*,#2586,.T.);
#3379=ORIENTED_EDGE('',*,*,#2587,.T.);
#3380=ORIENTED_EDGE('',*,*,#2588,.T.);
#3381=ORIENTED_EDGE('',*,*,#2589,.T.);
#3382=ORIENTED_EDGE('',*,*,#2590,.F.);
#3383=ORIENTED_EDGE('',*,*,#2591,.F.);
#3384=ORIENTED_EDGE('',*,*,#2589,.F.);
#3385=ORIENTED_EDGE('',*,*,#2592,.F.);
#3386=ORIENTED_EDGE('',*,*,#2578,.F.);
#3387=ORIENTED_EDGE('',*,*,#2592,.T.);
#3388=ORIENTED_EDGE('',*,*,#2588,.F.);
#3389=ORIENTED_EDGE('',*,*,#2593,.F.);
#3390=ORIENTED_EDGE('',*,*,#2579,.F.);
#3391=ORIENTED_EDGE('',*,*,#2593,.T.);
#3392=ORIENTED_EDGE('',*,*,#2587,.F.);
#3393=ORIENTED_EDGE('',*,*,#2594,.F.);
#3394=ORIENTED_EDGE('',*,*,#2580,.F.);
#3395=ORIENTED_EDGE('',*,*,#2594,.T.);
#3396=ORIENTED_EDGE('',*,*,#2586,.F.);
#3397=ORIENTED_EDGE('',*,*,#2595,.F.);
#3398=ORIENTED_EDGE('',*,*,#2581,.F.);
#3399=ORIENTED_EDGE('',*,*,#2595,.T.);
#3400=ORIENTED_EDGE('',*,*,#2585,.F.);
#3401=ORIENTED_EDGE('',*,*,#2596,.F.);
#3402=ORIENTED_EDGE('',*,*,#2582,.F.);
#3403=ORIENTED_EDGE('',*,*,#2596,.T.);
#3404=ORIENTED_EDGE('',*,*,#2584,.F.);
#3405=ORIENTED_EDGE('',*,*,#2591,.T.);
#3406=ORIENTED_EDGE('',*,*,#2577,.F.);
#3407=ORIENTED_EDGE('',*,*,#2590,.T.);
#3408=ORIENTED_EDGE('',*,*,#2597,.T.);
#3409=ORIENTED_EDGE('',*,*,#2598,.T.);
#3410=ORIENTED_EDGE('',*,*,#2597,.F.);
#3411=ORIENTED_EDGE('',*,*,#2599,.F.);
#3412=ORIENTED_EDGE('',*,*,#2600,.T.);
#3413=ORIENTED_EDGE('',*,*,#2598,.F.);
#3414=ORIENTED_EDGE('',*,*,#2601,.T.);
#3415=ORIENTED_EDGE('',*,*,#2599,.T.);
#3416=ORIENTED_EDGE('',*,*,#2601,.F.);
#3417=ORIENTED_EDGE('',*,*,#2602,.F.);
#3418=ORIENTED_EDGE('',*,*,#2603,.T.);
#3419=ORIENTED_EDGE('',*,*,#2583,.T.);
#3420=ORIENTED_EDGE('',*,*,#2603,.F.);
#3421=ORIENTED_EDGE('',*,*,#2604,.F.);
#3422=ORIENTED_EDGE('',*,*,#2605,.T.);
#3423=ORIENTED_EDGE('',*,*,#2602,.T.);
#3424=ORIENTED_EDGE('',*,*,#2605,.F.);
#3425=ORIENTED_EDGE('',*,*,#2604,.T.);
#3426=ORIENTED_EDGE('',*,*,#2606,.F.);
#3427=ORIENTED_EDGE('',*,*,#2606,.T.);
#3428=ORIENTED_EDGE('',*,*,#2607,.T.);
#3429=ORIENTED_EDGE('',*,*,#2600,.F.);
#3430=ORIENTED_EDGE('',*,*,#2607,.F.);
#3431=ORIENTED_EDGE('',*,*,#2608,.F.);
#3432=ORIENTED_EDGE('',*,*,#2609,.F.);
#3433=ORIENTED_EDGE('',*,*,#2610,.T.);
#3434=ORIENTED_EDGE('',*,*,#2608,.T.);
#3435=ORIENTED_EDGE('',*,*,#2610,.F.);
#3436=ORIENTED_EDGE('',*,*,#2611,.F.);
#3437=ORIENTED_EDGE('',*,*,#2612,.T.);
#3438=ORIENTED_EDGE('',*,*,#2609,.T.);
#3439=ORIENTED_EDGE('',*,*,#2612,.F.);
#3440=ORIENTED_EDGE('',*,*,#2613,.F.);
#3441=ORIENTED_EDGE('',*,*,#2614,.T.);
#3442=ORIENTED_EDGE('',*,*,#2611,.T.);
#3443=ORIENTED_EDGE('',*,*,#2614,.F.);
#3444=ORIENTED_EDGE('',*,*,#2613,.T.);
#3445=ORIENTED_EDGE('',*,*,#2615,.F.);
#3446=ORIENTED_EDGE('',*,*,#2616,.F.);
#3447=ORIENTED_EDGE('',*,*,#2617,.T.);
#3448=ORIENTED_EDGE('',*,*,#2615,.T.);
#3449=ORIENTED_EDGE('',*,*,#2617,.F.);
#3450=ORIENTED_EDGE('',*,*,#2618,.F.);
#3451=ORIENTED_EDGE('',*,*,#2619,.T.);
#3452=ORIENTED_EDGE('',*,*,#2616,.T.);
#3453=ORIENTED_EDGE('',*,*,#2619,.F.);
#3454=ORIENTED_EDGE('',*,*,#2620,.F.);
#3455=ORIENTED_EDGE('',*,*,#2621,.T.);
#3456=ORIENTED_EDGE('',*,*,#2618,.T.);
#3457=ORIENTED_EDGE('',*,*,#2621,.F.);
#3458=ORIENTED_EDGE('',*,*,#2620,.T.);
#3459=ORIENTED_EDGE('',*,*,#2622,.T.);
#3460=ORIENTED_EDGE('',*,*,#2623,.T.);
#3461=ORIENTED_EDGE('',*,*,#2624,.T.);
#3462=ORIENTED_EDGE('',*,*,#2625,.F.);
#3463=ORIENTED_EDGE('',*,*,#2626,.T.);
#3464=ORIENTED_EDGE('',*,*,#2627,.T.);
#3465=ORIENTED_EDGE('',*,*,#2628,.T.);
#3466=ORIENTED_EDGE('',*,*,#2623,.F.);
#3467=ORIENTED_EDGE('',*,*,#2629,.T.);
#3468=ORIENTED_EDGE('',*,*,#2630,.T.);
#3469=ORIENTED_EDGE('',*,*,#2631,.T.);
#3470=ORIENTED_EDGE('',*,*,#2627,.F.);
#3471=ORIENTED_EDGE('',*,*,#2632,.T.);
#3472=ORIENTED_EDGE('',*,*,#2633,.T.);
#3473=ORIENTED_EDGE('',*,*,#2634,.T.);
#3474=ORIENTED_EDGE('',*,*,#2630,.F.);
#3475=ORIENTED_EDGE('',*,*,#2635,.T.);
#3476=ORIENTED_EDGE('',*,*,#2636,.T.);
#3477=ORIENTED_EDGE('',*,*,#2637,.T.);
#3478=ORIENTED_EDGE('',*,*,#2633,.F.);
#3479=ORIENTED_EDGE('',*,*,#2638,.T.);
#3480=ORIENTED_EDGE('',*,*,#2625,.T.);
#3481=ORIENTED_EDGE('',*,*,#2639,.T.);
#3482=ORIENTED_EDGE('',*,*,#2636,.F.);
#3483=ORIENTED_EDGE('',*,*,#2638,.F.);
#3484=ORIENTED_EDGE('',*,*,#2635,.F.);
#3485=ORIENTED_EDGE('',*,*,#2632,.F.);
#3486=ORIENTED_EDGE('',*,*,#2629,.F.);
#3487=ORIENTED_EDGE('',*,*,#2626,.F.);
#3488=ORIENTED_EDGE('',*,*,#2622,.F.);
#3489=ORIENTED_EDGE('',*,*,#2639,.F.);
#3490=ORIENTED_EDGE('',*,*,#2624,.F.);
#3491=ORIENTED_EDGE('',*,*,#2628,.F.);
#3492=ORIENTED_EDGE('',*,*,#2631,.F.);
#3493=ORIENTED_EDGE('',*,*,#2634,.F.);
#3494=ORIENTED_EDGE('',*,*,#2637,.F.);
#3495=ORIENTED_EDGE('',*,*,#2640,.F.);
#3496=ORIENTED_EDGE('',*,*,#2641,.F.);
#3497=ORIENTED_EDGE('',*,*,#2642,.F.);
#3498=ORIENTED_EDGE('',*,*,#2643,.T.);
#3499=ORIENTED_EDGE('',*,*,#2644,.F.);
#3500=ORIENTED_EDGE('',*,*,#2643,.F.);
#3501=ORIENTED_EDGE('',*,*,#2645,.F.);
#3502=ORIENTED_EDGE('',*,*,#2646,.T.);
#3503=ORIENTED_EDGE('',*,*,#2647,.F.);
#3504=ORIENTED_EDGE('',*,*,#2648,.F.);
#3505=ORIENTED_EDGE('',*,*,#2646,.F.);
#3506=ORIENTED_EDGE('',*,*,#2649,.F.);
#3507=ORIENTED_EDGE('',*,*,#2650,.T.);
#3508=ORIENTED_EDGE('',*,*,#2651,.F.);
#3509=ORIENTED_EDGE('',*,*,#2650,.F.);
#3510=ORIENTED_EDGE('',*,*,#2652,.F.);
#3511=ORIENTED_EDGE('',*,*,#2641,.T.);
#3512=ORIENTED_EDGE('',*,*,#2645,.T.);
#3513=ORIENTED_EDGE('',*,*,#2642,.T.);
#3514=ORIENTED_EDGE('',*,*,#2652,.T.);
#3515=ORIENTED_EDGE('',*,*,#2649,.T.);
#3516=ORIENTED_EDGE('',*,*,#2653,.F.);
#3517=ORIENTED_EDGE('',*,*,#2654,.T.);
#3518=ORIENTED_EDGE('',*,*,#2655,.F.);
#3519=ORIENTED_EDGE('',*,*,#2654,.F.);
#3520=ORIENTED_EDGE('',*,*,#2648,.T.);
#3521=ORIENTED_EDGE('',*,*,#2651,.T.);
#3522=ORIENTED_EDGE('',*,*,#2640,.T.);
#3523=ORIENTED_EDGE('',*,*,#2644,.T.);
#3524=ORIENTED_EDGE('',*,*,#2656,.T.);
#3525=ORIENTED_EDGE('',*,*,#2656,.F.);
#3526=ORIENTED_EDGE('',*,*,#2647,.T.);
#3527=ORIENTED_EDGE('',*,*,#2655,.T.);
#3528=ORIENTED_EDGE('',*,*,#2653,.T.);
#3529=ORIENTED_EDGE('',*,*,#2657,.F.);
#3530=ORIENTED_EDGE('',*,*,#2658,.T.);
#3531=ORIENTED_EDGE('',*,*,#2659,.F.);
#3532=ORIENTED_EDGE('',*,*,#2658,.F.);
#3533=ORIENTED_EDGE('',*,*,#2657,.T.);
#3534=ORIENTED_EDGE('',*,*,#2660,.T.);
#3535=ORIENTED_EDGE('',*,*,#2661,.F.);
#3536=ORIENTED_EDGE('',*,*,#2662,.F.);
#3537=ORIENTED_EDGE('',*,*,#2663,.T.);
#3538=ORIENTED_EDGE('',*,*,#2664,.F.);
#3539=ORIENTED_EDGE('',*,*,#2665,.F.);
#3540=ORIENTED_EDGE('',*,*,#2666,.T.);
#3541=ORIENTED_EDGE('',*,*,#2667,.F.);
#3542=ORIENTED_EDGE('',*,*,#2668,.F.);
#3543=ORIENTED_EDGE('',*,*,#2669,.T.);
#3544=ORIENTED_EDGE('',*,*,#2670,.F.);
#3545=ORIENTED_EDGE('',*,*,#2671,.F.);
#3546=ORIENTED_EDGE('',*,*,#2670,.T.);
#3547=ORIENTED_EDGE('',*,*,#2672,.F.);
#3548=ORIENTED_EDGE('',*,*,#2662,.T.);
#3549=ORIENTED_EDGE('',*,*,#2673,.T.);
#3550=ORIENTED_EDGE('',*,*,#2674,.F.);
#3551=ORIENTED_EDGE('',*,*,#2675,.F.);
#3552=ORIENTED_EDGE('',*,*,#2667,.T.);
#3553=ORIENTED_EDGE('',*,*,#2676,.F.);
#3554=ORIENTED_EDGE('',*,*,#2671,.T.);
#3555=ORIENTED_EDGE('',*,*,#2675,.T.);
#3556=ORIENTED_EDGE('',*,*,#2677,.F.);
#3557=ORIENTED_EDGE('',*,*,#2678,.F.);
#3558=ORIENTED_EDGE('',*,*,#2664,.T.);
#3559=ORIENTED_EDGE('',*,*,#2679,.F.);
#3560=ORIENTED_EDGE('',*,*,#2668,.T.);
#3561=ORIENTED_EDGE('',*,*,#2678,.T.);
#3562=ORIENTED_EDGE('',*,*,#2680,.F.);
#3563=ORIENTED_EDGE('',*,*,#2681,.F.);
#3564=ORIENTED_EDGE('',*,*,#2661,.T.);
#3565=ORIENTED_EDGE('',*,*,#2682,.F.);
#3566=ORIENTED_EDGE('',*,*,#2665,.T.);
#3567=ORIENTED_EDGE('',*,*,#2681,.T.);
#3568=ORIENTED_EDGE('',*,*,#2683,.F.);
#3569=ORIENTED_EDGE('',*,*,#2673,.F.);
#3570=ORIENTED_EDGE('',*,*,#2683,.T.);
#3571=ORIENTED_EDGE('',*,*,#2680,.T.);
#3572=ORIENTED_EDGE('',*,*,#2677,.T.);
#3573=ORIENTED_EDGE('',*,*,#2674,.T.);
#3574=ORIENTED_EDGE('',*,*,#2659,.T.);
#3575=ORIENTED_EDGE('',*,*,#2679,.T.);
#3576=ORIENTED_EDGE('',*,*,#2684,.T.);
#3577=ORIENTED_EDGE('',*,*,#2682,.T.);
#3578=ORIENTED_EDGE('',*,*,#2685,.T.);
#3579=ORIENTED_EDGE('',*,*,#2686,.T.);
#3580=ORIENTED_EDGE('',*,*,#2672,.T.);
#3581=ORIENTED_EDGE('',*,*,#2687,.T.);
#3582=ORIENTED_EDGE('',*,*,#2676,.T.);
#3583=ORIENTED_EDGE('',*,*,#2688,.T.);
#3584=ORIENTED_EDGE('',*,*,#2689,.T.);
#3585=ORIENTED_EDGE('',*,*,#2690,.T.);
#3586=ORIENTED_EDGE('',*,*,#2691,.F.);
#3587=ORIENTED_EDGE('',*,*,#2692,.F.);
#3588=ORIENTED_EDGE('',*,*,#2693,.T.);
#3589=ORIENTED_EDGE('',*,*,#2692,.T.);
#3590=ORIENTED_EDGE('',*,*,#2694,.F.);
#3591=ORIENTED_EDGE('',*,*,#2695,.F.);
#3592=ORIENTED_EDGE('',*,*,#2696,.T.);
#3593=ORIENTED_EDGE('',*,*,#2695,.T.);
#3594=ORIENTED_EDGE('',*,*,#2697,.F.);
#3595=ORIENTED_EDGE('',*,*,#2698,.F.);
#3596=ORIENTED_EDGE('',*,*,#2699,.T.);
#3597=ORIENTED_EDGE('',*,*,#2698,.T.);
#3598=ORIENTED_EDGE('',*,*,#2700,.F.);
#3599=ORIENTED_EDGE('',*,*,#2690,.F.);
#3600=ORIENTED_EDGE('',*,*,#2699,.F.);
#3601=ORIENTED_EDGE('',*,*,#2689,.F.);
#3602=ORIENTED_EDGE('',*,*,#2693,.F.);
#3603=ORIENTED_EDGE('',*,*,#2696,.F.);
#3604=ORIENTED_EDGE('',*,*,#2685,.F.);
#3605=ORIENTED_EDGE('',*,*,#2660,.F.);
#3606=ORIENTED_EDGE('',*,*,#2687,.F.);
#3607=ORIENTED_EDGE('',*,*,#2669,.F.);
#3608=ORIENTED_EDGE('',*,*,#2688,.F.);
#3609=ORIENTED_EDGE('',*,*,#2666,.F.);
#3610=ORIENTED_EDGE('',*,*,#2684,.F.);
#3611=ORIENTED_EDGE('',*,*,#2663,.F.);
#3612=ORIENTED_EDGE('',*,*,#2686,.F.);
#3613=ORIENTED_EDGE('',*,*,#2701,.T.);
#3614=ORIENTED_EDGE('',*,*,#2702,.T.);
#3615=ORIENTED_EDGE('',*,*,#2701,.F.);
#3616=ORIENTED_EDGE('',*,*,#2702,.F.);
#3617=ORIENTED_EDGE('',*,*,#2691,.T.);
#3618=ORIENTED_EDGE('',*,*,#2700,.T.);
#3619=ORIENTED_EDGE('',*,*,#2697,.T.);
#3620=ORIENTED_EDGE('',*,*,#2694,.T.);
#3621=ORIENTED_EDGE('',*,*,#2703,.F.);
#3622=ORIENTED_EDGE('',*,*,#2704,.F.);
#3623=ORIENTED_EDGE('',*,*,#2705,.F.);
#3624=ORIENTED_EDGE('',*,*,#2706,.T.);
#3625=ORIENTED_EDGE('',*,*,#2707,.F.);
#3626=ORIENTED_EDGE('',*,*,#2706,.F.);
#3627=ORIENTED_EDGE('',*,*,#2708,.F.);
#3628=ORIENTED_EDGE('',*,*,#2709,.T.);
#3629=ORIENTED_EDGE('',*,*,#2710,.F.);
#3630=ORIENTED_EDGE('',*,*,#2709,.F.);
#3631=ORIENTED_EDGE('',*,*,#2711,.F.);
#3632=ORIENTED_EDGE('',*,*,#2712,.T.);
#3633=ORIENTED_EDGE('',*,*,#2713,.F.);
#3634=ORIENTED_EDGE('',*,*,#2712,.F.);
#3635=ORIENTED_EDGE('',*,*,#2714,.F.);
#3636=ORIENTED_EDGE('',*,*,#2704,.T.);
#3637=ORIENTED_EDGE('',*,*,#2715,.T.);
#3638=ORIENTED_EDGE('',*,*,#2716,.T.);
#3639=ORIENTED_EDGE('',*,*,#2717,.F.);
#3640=ORIENTED_EDGE('',*,*,#2718,.F.);
#3641=ORIENTED_EDGE('',*,*,#2719,.T.);
#3642=ORIENTED_EDGE('',*,*,#2718,.T.);
#3643=ORIENTED_EDGE('',*,*,#2720,.F.);
#3644=ORIENTED_EDGE('',*,*,#2721,.F.);
#3645=ORIENTED_EDGE('',*,*,#2722,.T.);
#3646=ORIENTED_EDGE('',*,*,#2721,.T.);
#3647=ORIENTED_EDGE('',*,*,#2723,.F.);
#3648=ORIENTED_EDGE('',*,*,#2724,.F.);
#3649=ORIENTED_EDGE('',*,*,#2725,.T.);
#3650=ORIENTED_EDGE('',*,*,#2724,.T.);
#3651=ORIENTED_EDGE('',*,*,#2726,.F.);
#3652=ORIENTED_EDGE('',*,*,#2716,.F.);
#3653=ORIENTED_EDGE('',*,*,#2726,.T.);
#3654=ORIENTED_EDGE('',*,*,#2723,.T.);
#3655=ORIENTED_EDGE('',*,*,#2720,.T.);
#3656=ORIENTED_EDGE('',*,*,#2717,.T.);
#3657=ORIENTED_EDGE('',*,*,#2710,.T.);
#3658=ORIENTED_EDGE('',*,*,#2713,.T.);
#3659=ORIENTED_EDGE('',*,*,#2703,.T.);
#3660=ORIENTED_EDGE('',*,*,#2707,.T.);
#3661=ORIENTED_EDGE('',*,*,#2725,.F.);
#3662=ORIENTED_EDGE('',*,*,#2715,.F.);
#3663=ORIENTED_EDGE('',*,*,#2719,.F.);
#3664=ORIENTED_EDGE('',*,*,#2722,.F.);
#3665=ORIENTED_EDGE('',*,*,#2711,.T.);
#3666=ORIENTED_EDGE('',*,*,#2708,.T.);
#3667=ORIENTED_EDGE('',*,*,#2705,.T.);
#3668=ORIENTED_EDGE('',*,*,#2714,.T.);
#3669=ORIENTED_EDGE('',*,*,#2727,.F.);
#3670=ORIENTED_EDGE('',*,*,#2728,.T.);
#3671=ORIENTED_EDGE('',*,*,#2729,.T.);
#3672=ORIENTED_EDGE('',*,*,#2728,.F.);
#3673=ORIENTED_EDGE('',*,*,#2730,.F.);
#3674=ORIENTED_EDGE('',*,*,#2731,.T.);
#3675=ORIENTED_EDGE('',*,*,#2732,.T.);
#3676=ORIENTED_EDGE('',*,*,#2731,.F.);
#3677=ORIENTED_EDGE('',*,*,#2730,.T.);
#3678=ORIENTED_EDGE('',*,*,#2727,.T.);
#3679=ORIENTED_EDGE('',*,*,#2732,.F.);
#3680=ORIENTED_EDGE('',*,*,#2729,.F.);
#3681=ORIENTED_EDGE('',*,*,#2733,.T.);
#3682=ORIENTED_EDGE('',*,*,#2734,.T.);
#3683=ORIENTED_EDGE('',*,*,#2735,.F.);
#3684=ORIENTED_EDGE('',*,*,#2736,.F.);
#3685=ORIENTED_EDGE('',*,*,#2737,.T.);
#3686=ORIENTED_EDGE('',*,*,#2736,.T.);
#3687=ORIENTED_EDGE('',*,*,#2738,.F.);
#3688=ORIENTED_EDGE('',*,*,#2739,.F.);
#3689=ORIENTED_EDGE('',*,*,#2740,.T.);
#3690=ORIENTED_EDGE('',*,*,#2739,.T.);
#3691=ORIENTED_EDGE('',*,*,#2741,.F.);
#3692=ORIENTED_EDGE('',*,*,#2742,.F.);
#3693=ORIENTED_EDGE('',*,*,#2743,.T.);
#3694=ORIENTED_EDGE('',*,*,#2742,.T.);
#3695=ORIENTED_EDGE('',*,*,#2744,.F.);
#3696=ORIENTED_EDGE('',*,*,#2734,.F.);
#3697=ORIENTED_EDGE('',*,*,#2744,.T.);
#3698=ORIENTED_EDGE('',*,*,#2741,.T.);
#3699=ORIENTED_EDGE('',*,*,#2738,.T.);
#3700=ORIENTED_EDGE('',*,*,#2735,.T.);
#3701=ORIENTED_EDGE('',*,*,#2743,.F.);
#3702=ORIENTED_EDGE('',*,*,#2733,.F.);
#3703=ORIENTED_EDGE('',*,*,#2737,.F.);
#3704=ORIENTED_EDGE('',*,*,#2740,.F.);
#3705=ORIENTED_EDGE('',*,*,#2745,.T.);
#3706=ORIENTED_EDGE('',*,*,#2746,.T.);
#3707=ORIENTED_EDGE('',*,*,#2747,.T.);
#3708=ORIENTED_EDGE('',*,*,#2748,.F.);
#3709=ORIENTED_EDGE('',*,*,#2749,.T.);
#3710=ORIENTED_EDGE('',*,*,#2750,.T.);
#3711=ORIENTED_EDGE('',*,*,#2751,.T.);
#3712=ORIENTED_EDGE('',*,*,#2746,.F.);
#3713=ORIENTED_EDGE('',*,*,#2752,.T.);
#3714=ORIENTED_EDGE('',*,*,#2753,.T.);
#3715=ORIENTED_EDGE('',*,*,#2754,.T.);
#3716=ORIENTED_EDGE('',*,*,#2750,.F.);
#3717=ORIENTED_EDGE('',*,*,#2755,.T.);
#3718=ORIENTED_EDGE('',*,*,#2756,.T.);
#3719=ORIENTED_EDGE('',*,*,#2757,.T.);
#3720=ORIENTED_EDGE('',*,*,#2753,.F.);
#3721=ORIENTED_EDGE('',*,*,#2758,.T.);
#3722=ORIENTED_EDGE('',*,*,#2759,.T.);
#3723=ORIENTED_EDGE('',*,*,#2760,.T.);
#3724=ORIENTED_EDGE('',*,*,#2756,.F.);
#3725=ORIENTED_EDGE('',*,*,#2761,.T.);
#3726=ORIENTED_EDGE('',*,*,#2748,.T.);
#3727=ORIENTED_EDGE('',*,*,#2762,.T.);
#3728=ORIENTED_EDGE('',*,*,#2759,.F.);
#3729=ORIENTED_EDGE('',*,*,#2761,.F.);
#3730=ORIENTED_EDGE('',*,*,#2758,.F.);
#3731=ORIENTED_EDGE('',*,*,#2755,.F.);
#3732=ORIENTED_EDGE('',*,*,#2752,.F.);
#3733=ORIENTED_EDGE('',*,*,#2749,.F.);
#3734=ORIENTED_EDGE('',*,*,#2745,.F.);
#3735=ORIENTED_EDGE('',*,*,#2762,.F.);
#3736=ORIENTED_EDGE('',*,*,#2747,.F.);
#3737=ORIENTED_EDGE('',*,*,#2751,.F.);
#3738=ORIENTED_EDGE('',*,*,#2754,.F.);
#3739=ORIENTED_EDGE('',*,*,#2757,.F.);
#3740=ORIENTED_EDGE('',*,*,#2760,.F.);
#3741=ORIENTED_EDGE('',*,*,#2763,.F.);
#3742=ORIENTED_EDGE('',*,*,#2764,.F.);
#3743=ORIENTED_EDGE('',*,*,#2765,.F.);
#3744=ORIENTED_EDGE('',*,*,#2766,.T.);
#3745=ORIENTED_EDGE('',*,*,#2764,.T.);
#3746=ORIENTED_EDGE('',*,*,#2766,.F.);
#3747=ORIENTED_EDGE('',*,*,#2767,.F.);
#3748=ORIENTED_EDGE('',*,*,#2768,.T.);
#3749=ORIENTED_EDGE('',*,*,#2765,.T.);
#3750=ORIENTED_EDGE('',*,*,#2768,.F.);
#3751=ORIENTED_EDGE('',*,*,#2769,.F.);
#3752=ORIENTED_EDGE('',*,*,#2770,.T.);
#3753=ORIENTED_EDGE('',*,*,#2767,.T.);
#3754=ORIENTED_EDGE('',*,*,#2770,.F.);
#3755=ORIENTED_EDGE('',*,*,#2769,.T.);
#3756=ORIENTED_EDGE('',*,*,#2771,.F.);
#3757=ORIENTED_EDGE('',*,*,#2772,.F.);
#3758=ORIENTED_EDGE('',*,*,#2773,.T.);
#3759=ORIENTED_EDGE('',*,*,#2771,.T.);
#3760=ORIENTED_EDGE('',*,*,#2773,.F.);
#3761=ORIENTED_EDGE('',*,*,#2763,.T.);
#3762=ORIENTED_EDGE('',*,*,#2774,.T.);
#3763=ORIENTED_EDGE('',*,*,#2772,.T.);
#3764=ORIENTED_EDGE('',*,*,#2774,.F.);
#3765=CYLINDRICAL_SURFACE('',#4401,0.165);
#3766=CYLINDRICAL_SURFACE('',#4405,0.165);
#3767=CYLINDRICAL_SURFACE('',#4409,0.275);
#3768=CYLINDRICAL_SURFACE('',#4412,0.275);
#3769=CYLINDRICAL_SURFACE('',#4415,0.275);
#3770=CYLINDRICAL_SURFACE('',#4418,0.275);
#3771=CYLINDRICAL_SURFACE('',#4421,0.7);
#3772=CYLINDRICAL_SURFACE('',#4427,0.93);
#3773=CYLINDRICAL_SURFACE('',#4430,1.3);
#3774=CYLINDRICAL_SURFACE('',#4447,0.75);
#3775=CYLINDRICAL_SURFACE('',#4449,1.3);
#3776=CYLINDRICAL_SURFACE('',#4455,0.165);
#3777=CYLINDRICAL_SURFACE('',#4459,0.165);
#3778=CYLINDRICAL_SURFACE('',#4463,0.275);
#3779=CYLINDRICAL_SURFACE('',#4466,0.275);
#3780=CYLINDRICAL_SURFACE('',#4469,0.275);
#3781=CYLINDRICAL_SURFACE('',#4472,0.275);
#3782=CYLINDRICAL_SURFACE('',#4475,0.7);
#3783=CYLINDRICAL_SURFACE('',#4481,0.93);
#3784=CYLINDRICAL_SURFACE('',#4484,1.3);
#3785=CYLINDRICAL_SURFACE('',#4501,0.75);
#3786=CYLINDRICAL_SURFACE('',#4503,1.3);
#3787=CYLINDRICAL_SURFACE('',#4509,0.275);
#3788=CYLINDRICAL_SURFACE('',#4512,0.275);
#3789=CYLINDRICAL_SURFACE('',#4515,0.275);
#3790=CYLINDRICAL_SURFACE('',#4518,0.275);
#3791=CYLINDRICAL_SURFACE('',#4529,1.6);
#3792=CYLINDRICAL_SURFACE('',#4539,1.2);
#3793=CYLINDRICAL_SURFACE('',#4543,0.405);
#3794=CYLINDRICAL_SURFACE('',#4545,0.7);
#3795=CYLINDRICAL_SURFACE('',#4553,0.61);
#3796=CYLINDRICAL_SURFACE('',#4558,0.405);
#3797=CYLINDRICAL_SURFACE('',#4560,1.);
#3798=CYLINDRICAL_SURFACE('',#4566,0.3);
#3799=CYLINDRICAL_SURFACE('',#4570,0.3);
#3800=CYLINDRICAL_SURFACE('',#4574,0.225);
#3801=CYLINDRICAL_SURFACE('',#4577,0.225);
#3802=CYLINDRICAL_SURFACE('',#4580,0.225);
#3803=CYLINDRICAL_SURFACE('',#4583,0.225);
#3804=CYLINDRICAL_SURFACE('',#4586,1.01);
#3805=CYLINDRICAL_SURFACE('',#4596,0.225);
#3806=CYLINDRICAL_SURFACE('',#4599,0.4);
#3807=CYLINDRICAL_SURFACE('',#4605,0.225);
#3808=CYLINDRICAL_SURFACE('',#4608,0.4);
#3809=CYLINDRICAL_SURFACE('',#4614,0.225);
#3810=CYLINDRICAL_SURFACE('',#4617,0.4);
#3811=CYLINDRICAL_SURFACE('',#4623,0.225);
#3812=CYLINDRICAL_SURFACE('',#4626,0.4);
#3813=CYLINDRICAL_SURFACE('',#4632,0.3);
#3814=CYLINDRICAL_SURFACE('',#4638,0.3);
#3815=CYLINDRICAL_SURFACE('',#4655,0.25);
#3816=CYLINDRICAL_SURFACE('',#4662,0.425);
#3817=CYLINDRICAL_SURFACE('',#4670,0.24505);
#3818=CYLINDRICAL_SURFACE('',#4675,0.265);
#3819=CYLINDRICAL_SURFACE('',#4679,0.5);
#3820=CYLINDRICAL_SURFACE('',#4690,0.2117);
#3821=CYLINDRICAL_SURFACE('',#4709,1.065);
#3822=CYLINDRICAL_SURFACE('',#4715,1.065);
#3823=CYLINDRICAL_SURFACE('',#4721,0.79);
#3824=CYLINDRICAL_SURFACE('',#4727,0.35);
#3825=CYLINDRICAL_SURFACE('',#4735,0.1954);
#3826=CYLINDRICAL_SURFACE('',#4797,0.75);
#3827=CYLINDRICAL_SURFACE('',#4803,0.165);
#3828=CYLINDRICAL_SURFACE('',#4834,0.4);
#3829=CYLINDRICAL_SURFACE('',#4849,0.225);
#3830=CYLINDRICAL_SURFACE('',#4852,0.6);
#3831=CYLINDRICAL_SURFACE('',#4879,0.35);
#3832=CYLINDRICAL_SURFACE('',#4887,0.1954);
#3833=ADVANCED_FACE('',(#579),#3765,.F.);
#3834=ADVANCED_FACE('',(#580),#419,.T.);
#3835=ADVANCED_FACE('',(#581),#3766,.F.);
#3836=ADVANCED_FACE('',(#582),#420,.T.);
#3837=ADVANCED_FACE('',(#583),#3767,.F.);
#3838=ADVANCED_FACE('',(#584),#3768,.F.);
#3839=ADVANCED_FACE('',(#585),#3769,.F.);
#3840=ADVANCED_FACE('',(#586),#3770,.F.);
#3841=ADVANCED_FACE('',(#587),#3771,.F.);
#3842=ADVANCED_FACE('',(#588),#421,.T.);
#3843=ADVANCED_FACE('',(#589,#331,#332),#422,.T.);
#3844=ADVANCED_FACE('',(#590),#3772,.F.);
#3845=ADVANCED_FACE('',(#591),#3773,.F.);
#3846=ADVANCED_FACE('',(#592,#333),#423,.F.);
#3847=ADVANCED_FACE('',(#593,#334),#424,.T.);
#3848=ADVANCED_FACE('',(#594,#335),#326,.F.);
#3849=ADVANCED_FACE('',(#595,#336,#337,#338,#339),#425,.T.);
#3850=ADVANCED_FACE('',(#596),#426,.T.);
#3851=ADVANCED_FACE('',(#597,#340,#341,#342,#343,#344),#427,.T.);
#3852=ADVANCED_FACE('',(#598),#428,.T.);
#3853=ADVANCED_FACE('',(#599),#429,.F.);
#3854=ADVANCED_FACE('',(#600,#345),#327,.F.);
#3855=ADVANCED_FACE('',(#601),#3774,.F.);
#3856=ADVANCED_FACE('',(#602),#3775,.T.);
#3857=ADVANCED_FACE('',(#603,#346),#430,.T.);
#3858=ADVANCED_FACE('',(#604,#347),#431,.F.);
#3859=ADVANCED_FACE('',(#605),#3776,.F.);
#3860=ADVANCED_FACE('',(#606),#432,.T.);
#3861=ADVANCED_FACE('',(#607),#3777,.F.);
#3862=ADVANCED_FACE('',(#608),#433,.T.);
#3863=ADVANCED_FACE('',(#609),#3778,.F.);
#3864=ADVANCED_FACE('',(#610),#3779,.F.);
#3865=ADVANCED_FACE('',(#611),#3780,.F.);
#3866=ADVANCED_FACE('',(#612),#3781,.F.);
#3867=ADVANCED_FACE('',(#613),#3782,.F.);
#3868=ADVANCED_FACE('',(#614),#434,.T.);
#3869=ADVANCED_FACE('',(#615,#348,#349),#435,.T.);
#3870=ADVANCED_FACE('',(#616),#3783,.F.);
#3871=ADVANCED_FACE('',(#617),#3784,.F.);
#3872=ADVANCED_FACE('',(#618,#350),#436,.F.);
#3873=ADVANCED_FACE('',(#619,#351),#437,.T.);
#3874=ADVANCED_FACE('',(#620,#352),#328,.F.);
#3875=ADVANCED_FACE('',(#621,#353,#354,#355,#356,#357),#438,.T.);
#3876=ADVANCED_FACE('',(#622),#439,.T.);
#3877=ADVANCED_FACE('',(#623,#358,#359,#360,#361),#440,.T.);
#3878=ADVANCED_FACE('',(#624),#441,.T.);
#3879=ADVANCED_FACE('',(#625),#442,.F.);
#3880=ADVANCED_FACE('',(#626,#362),#329,.F.);
#3881=ADVANCED_FACE('',(#627),#3785,.F.);
#3882=ADVANCED_FACE('',(#628),#3786,.T.);
#3883=ADVANCED_FACE('',(#629,#363),#443,.T.);
#3884=ADVANCED_FACE('',(#630,#364),#444,.F.);
#3885=ADVANCED_FACE('',(#631),#3787,.F.);
#3886=ADVANCED_FACE('',(#632),#3788,.F.);
#3887=ADVANCED_FACE('',(#633),#3789,.F.);
#3888=ADVANCED_FACE('',(#634),#3790,.F.);
#3889=ADVANCED_FACE('',(#635),#445,.F.);
#3890=ADVANCED_FACE('',(#636),#446,.F.);
#3891=ADVANCED_FACE('',(#637),#447,.F.);
#3892=ADVANCED_FACE('',(#638),#448,.F.);
#3893=ADVANCED_FACE('',(#639,#365,#366,#367,#368),#449,.T.);
#3894=ADVANCED_FACE('',(#640),#450,.T.);
#3895=ADVANCED_FACE('',(#641),#451,.T.);
#3896=ADVANCED_FACE('',(#642),#3791,.F.);
#3897=ADVANCED_FACE('',(#643),#452,.T.);
#3898=ADVANCED_FACE('',(#644),#453,.T.);
#3899=ADVANCED_FACE('',(#645),#454,.T.);
#3900=ADVANCED_FACE('',(#646,#369,#370,#371,#372),#455,.F.);
#3901=ADVANCED_FACE('',(#647,#373),#456,.F.);
#3902=ADVANCED_FACE('',(#648),#3792,.T.);
#3903=ADVANCED_FACE('',(#649,#374),#457,.T.);
#3904=ADVANCED_FACE('',(#650),#3793,.F.);
#3905=ADVANCED_FACE('',(#651),#3794,.T.);
#3906=ADVANCED_FACE('',(#652,#375),#458,.F.);
#3907=ADVANCED_FACE('',(#653),#224,.T.);
#3908=ADVANCED_FACE('',(#654),#3795,.F.);
#3909=ADVANCED_FACE('',(#655,#376),#459,.F.);
#3910=ADVANCED_FACE('',(#656),#3796,.F.);
#3911=ADVANCED_FACE('',(#657),#3797,.T.);
#3912=ADVANCED_FACE('',(#658,#377),#460,.T.);
#3913=ADVANCED_FACE('',(#659,#378),#461,.F.);
#3914=ADVANCED_FACE('',(#660),#3798,.F.);
#3915=ADVANCED_FACE('',(#661),#462,.T.);
#3916=ADVANCED_FACE('',(#662),#3799,.F.);
#3917=ADVANCED_FACE('',(#663),#463,.T.);
#3918=ADVANCED_FACE('',(#664),#3800,.F.);
#3919=ADVANCED_FACE('',(#665),#3801,.F.);
#3920=ADVANCED_FACE('',(#666),#3802,.F.);
#3921=ADVANCED_FACE('',(#667),#3803,.F.);
#3922=ADVANCED_FACE('',(#668),#3804,.F.);
#3923=ADVANCED_FACE('',(#669),#464,.T.);
#3924=ADVANCED_FACE('',(#670),#465,.T.);
#3925=ADVANCED_FACE('',(#671),#466,.T.);
#3926=ADVANCED_FACE('',(#672),#467,.T.);
#3927=ADVANCED_FACE('',(#673,#379,#380,#381,#382,#383,#384,#385),#468,.T.);
#3928=ADVANCED_FACE('',(#674,#386,#387,#388,#389,#390),#469,.F.);
#3929=ADVANCED_FACE('',(#675),#3805,.F.);
#3930=ADVANCED_FACE('',(#676),#3806,.T.);
#3931=ADVANCED_FACE('',(#677,#391),#470,.T.);
#3932=ADVANCED_FACE('',(#678,#392),#471,.F.);
#3933=ADVANCED_FACE('',(#679),#3807,.F.);
#3934=ADVANCED_FACE('',(#680),#3808,.T.);
#3935=ADVANCED_FACE('',(#681,#393),#472,.T.);
#3936=ADVANCED_FACE('',(#682,#394),#473,.F.);
#3937=ADVANCED_FACE('',(#683),#3809,.F.);
#3938=ADVANCED_FACE('',(#684),#3810,.T.);
#3939=ADVANCED_FACE('',(#685,#395),#474,.T.);
#3940=ADVANCED_FACE('',(#686,#396),#475,.F.);
#3941=ADVANCED_FACE('',(#687),#3811,.F.);
#3942=ADVANCED_FACE('',(#688),#3812,.T.);
#3943=ADVANCED_FACE('',(#689,#397),#476,.T.);
#3944=ADVANCED_FACE('',(#690,#398),#477,.F.);
#3945=ADVANCED_FACE('',(#691),#3813,.T.);
#3946=ADVANCED_FACE('',(#692),#478,.T.);
#3947=ADVANCED_FACE('',(#693),#479,.F.);
#3948=ADVANCED_FACE('',(#694),#3814,.T.);
#3949=ADVANCED_FACE('',(#695),#480,.T.);
#3950=ADVANCED_FACE('',(#696),#481,.F.);
#3951=ADVANCED_FACE('',(#697),#482,.F.);
#3952=ADVANCED_FACE('',(#698),#483,.F.);
#3953=ADVANCED_FACE('',(#699),#484,.F.);
#3954=ADVANCED_FACE('',(#700),#485,.F.);
#3955=ADVANCED_FACE('',(#701),#486,.F.);
#3956=ADVANCED_FACE('',(#702),#487,.F.);
#3957=ADVANCED_FACE('',(#703),#488,.F.);
#3958=ADVANCED_FACE('',(#704),#489,.F.);
#3959=ADVANCED_FACE('',(#705,#399),#490,.T.);
#3960=ADVANCED_FACE('',(#706),#3815,.T.);
#3961=ADVANCED_FACE('',(#707),#491,.F.);
#3962=ADVANCED_FACE('',(#708),#492,.T.);
#3963=ADVANCED_FACE('',(#709),#203,.T.);
#3964=ADVANCED_FACE('',(#710),#3816,.T.);
#3965=ADVANCED_FACE('',(#711),#204,.T.);
#3966=ADVANCED_FACE('',(#712,#400),#493,.T.);
#3967=ADVANCED_FACE('',(#713),#205,.T.);
#3968=ADVANCED_FACE('',(#714),#3817,.T.);
#3969=ADVANCED_FACE('',(#715),#206,.F.);
#3970=ADVANCED_FACE('',(#716),#3818,.F.);
#3971=ADVANCED_FACE('',(#717,#401),#494,.T.);
#3972=ADVANCED_FACE('',(#718),#3819,.T.);
#3973=ADVANCED_FACE('',(#719,#402),#495,.F.);
#3974=ADVANCED_FACE('',(#720),#207,.T.);
#3975=ADVANCED_FACE('',(#721),#208,.T.);
#3976=ADVANCED_FACE('',(#722),#496,.T.);
#3977=ADVANCED_FACE('',(#723),#497,.T.);
#3978=ADVANCED_FACE('',(#724),#498,.T.);
#3979=ADVANCED_FACE('',(#725),#3820,.F.);
#3980=ADVANCED_FACE('',(#726),#499,.T.);
#3981=ADVANCED_FACE('',(#727),#500,.T.);
#3982=ADVANCED_FACE('',(#728),#501,.T.);
#3983=ADVANCED_FACE('',(#729,#403),#502,.T.);
#3984=ADVANCED_FACE('',(#730,#404),#503,.F.);
#3985=ADVANCED_FACE('',(#731,#405),#504,.F.);
#3986=ADVANCED_FACE('',(#732,#406),#505,.T.);
#3987=ADVANCED_FACE('',(#733),#506,.T.);
#3988=ADVANCED_FACE('',(#734),#507,.T.);
#3989=ADVANCED_FACE('',(#735),#508,.T.);
#3990=ADVANCED_FACE('',(#736),#509,.T.);
#3991=ADVANCED_FACE('',(#737),#510,.T.);
#3992=ADVANCED_FACE('',(#738),#511,.T.);
#3993=ADVANCED_FACE('',(#739),#3821,.T.);
#3994=ADVANCED_FACE('',(#740,#407),#512,.T.);
#3995=ADVANCED_FACE('',(#741),#209,.T.);
#3996=ADVANCED_FACE('',(#742),#3822,.T.);
#3997=ADVANCED_FACE('',(#743),#210,.T.);
#3998=ADVANCED_FACE('',(#744,#408),#513,.T.);
#3999=ADVANCED_FACE('',(#745),#3823,.F.);
#4000=ADVANCED_FACE('',(#746),#514,.T.);
#4001=ADVANCED_FACE('',(#747),#211,.T.);
#4002=ADVANCED_FACE('',(#748),#3824,.T.);
#4003=ADVANCED_FACE('',(#749),#212,.T.);
#4004=ADVANCED_FACE('',(#750,#409),#515,.T.);
#4005=ADVANCED_FACE('',(#751),#213,.T.);
#4006=ADVANCED_FACE('',(#752),#3825,.T.);
#4007=ADVANCED_FACE('',(#753),#214,.T.);
#4008=ADVANCED_FACE('',(#754),#516,.T.);
#4009=ADVANCED_FACE('',(#755),#517,.F.);
#4010=ADVANCED_FACE('',(#756),#518,.F.);
#4011=ADVANCED_FACE('',(#757),#519,.F.);
#4012=ADVANCED_FACE('',(#758),#520,.F.);
#4013=ADVANCED_FACE('',(#759),#521,.F.);
#4014=ADVANCED_FACE('',(#760),#522,.F.);
#4015=ADVANCED_FACE('',(#761),#523,.F.);
#4016=ADVANCED_FACE('',(#762),#524,.F.);
#4017=ADVANCED_FACE('',(#763),#525,.F.);
#4018=ADVANCED_FACE('',(#764),#526,.F.);
#4019=ADVANCED_FACE('',(#765),#527,.F.);
#4020=ADVANCED_FACE('',(#766),#528,.F.);
#4021=ADVANCED_FACE('',(#767),#529,.T.);
#4022=ADVANCED_FACE('',(#768),#3826,.F.);
#4023=ADVANCED_FACE('',(#769,#410,#411),#330,.T.);
#4024=ADVANCED_FACE('',(#770),#3827,.F.);
#4025=ADVANCED_FACE('',(#771),#530,.T.);
#4026=ADVANCED_FACE('',(#772),#531,.F.);
#4027=ADVANCED_FACE('',(#773),#532,.F.);
#4028=ADVANCED_FACE('',(#774),#533,.F.);
#4029=ADVANCED_FACE('',(#775),#534,.F.);
#4030=ADVANCED_FACE('',(#776),#535,.T.);
#4031=ADVANCED_FACE('',(#777),#536,.T.);
#4032=ADVANCED_FACE('',(#778),#537,.T.);
#4033=ADVANCED_FACE('',(#779),#538,.T.);
#4034=ADVANCED_FACE('',(#780,#412),#539,.T.);
#4035=ADVANCED_FACE('',(#781),#540,.T.);
#4036=ADVANCED_FACE('',(#782),#541,.T.);
#4037=ADVANCED_FACE('',(#783),#542,.T.);
#4038=ADVANCED_FACE('',(#784),#543,.T.);
#4039=ADVANCED_FACE('',(#785),#544,.T.);
#4040=ADVANCED_FACE('',(#786),#545,.T.);
#4041=ADVANCED_FACE('',(#787),#546,.T.);
#4042=ADVANCED_FACE('',(#788),#547,.T.);
#4043=ADVANCED_FACE('',(#789),#548,.F.);
#4044=ADVANCED_FACE('',(#790),#3828,.T.);
#4045=ADVANCED_FACE('',(#791,#413),#549,.F.);
#4046=ADVANCED_FACE('',(#792),#550,.F.);
#4047=ADVANCED_FACE('',(#793),#551,.F.);
#4048=ADVANCED_FACE('',(#794),#552,.F.);
#4049=ADVANCED_FACE('',(#795),#553,.F.);
#4050=ADVANCED_FACE('',(#796),#554,.T.);
#4051=ADVANCED_FACE('',(#797),#555,.T.);
#4052=ADVANCED_FACE('',(#798),#556,.T.);
#4053=ADVANCED_FACE('',(#799),#557,.T.);
#4054=ADVANCED_FACE('',(#800,#414),#558,.T.);
#4055=ADVANCED_FACE('',(#801,#415),#559,.F.);
#4056=ADVANCED_FACE('',(#802),#3829,.F.);
#4057=ADVANCED_FACE('',(#803),#3830,.T.);
#4058=ADVANCED_FACE('',(#804,#416),#560,.T.);
#4059=ADVANCED_FACE('',(#805,#417),#561,.F.);
#4060=ADVANCED_FACE('',(#806),#562,.T.);
#4061=ADVANCED_FACE('',(#807),#563,.T.);
#4062=ADVANCED_FACE('',(#808),#564,.T.);
#4063=ADVANCED_FACE('',(#809),#565,.T.);
#4064=ADVANCED_FACE('',(#810),#566,.T.);
#4065=ADVANCED_FACE('',(#811),#567,.F.);
#4066=ADVANCED_FACE('',(#812),#568,.F.);
#4067=ADVANCED_FACE('',(#813),#569,.F.);
#4068=ADVANCED_FACE('',(#814),#570,.F.);
#4069=ADVANCED_FACE('',(#815),#571,.F.);
#4070=ADVANCED_FACE('',(#816),#572,.F.);
#4071=ADVANCED_FACE('',(#817),#573,.F.);
#4072=ADVANCED_FACE('',(#818),#574,.F.);
#4073=ADVANCED_FACE('',(#819),#575,.F.);
#4074=ADVANCED_FACE('',(#820),#576,.F.);
#4075=ADVANCED_FACE('',(#821),#577,.T.);
#4076=ADVANCED_FACE('',(#822),#215,.T.);
#4077=ADVANCED_FACE('',(#823),#3831,.T.);
#4078=ADVANCED_FACE('',(#824),#216,.T.);
#4079=ADVANCED_FACE('',(#825,#418),#578,.T.);
#4080=ADVANCED_FACE('',(#826),#217,.T.);
#4081=ADVANCED_FACE('',(#827),#3832,.T.);
#4082=CLOSED_SHELL('',(#3833,#3834,#3835,#3836,#3837,#3838,#3839,#3840,
#3841,#3842,#3843,#3844,#3845,#3846,#3847,#3848,#3849,#3850,#3851,#3852,
#3853));
#4083=CLOSED_SHELL('',(#3854,#3855,#3856,#3857,#3858));
#4084=CLOSED_SHELL('',(#3859,#3860,#3861,#3862,#3863,#3864,#3865,#3866,
#3867,#3868,#3869,#3870,#3871,#3872,#3873,#3874,#3875,#3876,#3877,#3878,
#3879));
#4085=CLOSED_SHELL('',(#3880,#3881,#3882,#3883,#3884));
#4086=CLOSED_SHELL('',(#3885,#3886,#3887,#3888,#3889,#3890,#3891,#3892,
#3893,#3894,#3895,#3896,#3897,#3898,#3899,#3900));
#4087=CLOSED_SHELL('',(#3901,#3902,#3903,#3904,#3905,#3906));
#4088=CLOSED_SHELL('',(#3907));
#4089=CLOSED_SHELL('',(#3908,#3909,#3910,#3911,#3912,#3913));
#4090=CLOSED_SHELL('',(#3914,#3915,#3916,#3917,#3918,#3919,#3920,#3921,
#3922,#3923,#3924,#3925,#3926,#3927,#3928));
#4091=CLOSED_SHELL('',(#3929,#3930,#3931,#3932));
#4092=CLOSED_SHELL('',(#3933,#3934,#3935,#3936));
#4093=CLOSED_SHELL('',(#3937,#3938,#3939,#3940));
#4094=CLOSED_SHELL('',(#3941,#3942,#3943,#3944));
#4095=CLOSED_SHELL('',(#3945,#3946,#3947));
#4096=CLOSED_SHELL('',(#3948,#3949,#3950));
#4097=CLOSED_SHELL('',(#3951,#3952,#3953,#3954,#3955,#3956,#3957,#3958));
#4098=CLOSED_SHELL('',(#3959,#3960,#3961,#3962,#3963,#3964,#3965,#3966,
#3967,#3968));
#4099=CLOSED_SHELL('',(#3969,#3970,#3971,#3972,#3973));
#4100=CLOSED_SHELL('',(#3974,#3975,#3976,#3977,#3978,#3979,#3980,#3981,
#3982,#3983,#3984));
#4101=CLOSED_SHELL('',(#3985,#3986,#3987,#3988,#3989,#3990,#3991,#3992,
#3993,#3994,#3995,#3996,#3997,#3998,#3999));
#4102=CLOSED_SHELL('',(#4000,#4001,#4002,#4003,#4004,#4005,#4006,#4007,
#4008));
#4103=CLOSED_SHELL('',(#4009,#4010,#4011,#4012,#4013,#4014,#4015,#4016));
#4104=CLOSED_SHELL('',(#4017,#4018,#4019,#4020,#4021,#4022,#4023));
#4105=CLOSED_SHELL('',(#4024,#4025,#4026,#4027,#4028,#4029,#4030,#4031,
#4032,#4033,#4034,#4035,#4036,#4037,#4038,#4039,#4040,#4041,#4042,#4043,
#4044,#4045));
#4106=CLOSED_SHELL('',(#4046,#4047,#4048,#4049,#4050,#4051,#4052,#4053,
#4054,#4055));
#4107=CLOSED_SHELL('',(#4056,#4057,#4058,#4059));
#4108=CLOSED_SHELL('',(#4060,#4061,#4062,#4063,#4064,#4065));
#4109=CLOSED_SHELL('',(#4066,#4067,#4068,#4069,#4070,#4071,#4072,#4073));
#4110=CLOSED_SHELL('',(#4074,#4075,#4076,#4077,#4078,#4079,#4080,#4081));
#4111=DERIVED_UNIT_ELEMENT(#4163,1.);
#4112=DERIVED_UNIT_ELEMENT(#7427,-3.);
#4113=DERIVED_UNIT_ELEMENT(#4163,1.);
#4114=DERIVED_UNIT_ELEMENT(#7427,-3.);
#4115=DERIVED_UNIT_ELEMENT(#4163,1.);
#4116=DERIVED_UNIT_ELEMENT(#7427,-3.);
#4117=DERIVED_UNIT_ELEMENT(#4163,1.);
#4118=DERIVED_UNIT_ELEMENT(#7427,-3.);
#4119=DERIVED_UNIT_ELEMENT(#4163,1.);
#4120=DERIVED_UNIT_ELEMENT(#7427,-3.);
#4121=DERIVED_UNIT_ELEMENT(#4163,1.);
#4122=DERIVED_UNIT_ELEMENT(#7427,-3.);
#4123=DERIVED_UNIT_ELEMENT(#4163,1.);
#4124=DERIVED_UNIT_ELEMENT(#7427,-3.);
#4125=DERIVED_UNIT_ELEMENT(#4163,1.);
#4126=DERIVED_UNIT_ELEMENT(#7427,-3.);
#4127=DERIVED_UNIT_ELEMENT(#4163,1.);
#4128=DERIVED_UNIT_ELEMENT(#7427,-3.);
#4129=DERIVED_UNIT_ELEMENT(#4163,1.);
#4130=DERIVED_UNIT_ELEMENT(#7427,-3.);
#4131=DERIVED_UNIT_ELEMENT(#4163,1.);
#4132=DERIVED_UNIT_ELEMENT(#7427,-3.);
#4133=DERIVED_UNIT_ELEMENT(#4163,1.);
#4134=DERIVED_UNIT_ELEMENT(#7427,-3.);
#4135=DERIVED_UNIT_ELEMENT(#4163,1.);
#4136=DERIVED_UNIT_ELEMENT(#7427,-3.);
#4137=DERIVED_UNIT_ELEMENT(#4163,1.);
#4138=DERIVED_UNIT_ELEMENT(#7427,-3.);
#4139=DERIVED_UNIT_ELEMENT(#4163,1.);
#4140=DERIVED_UNIT_ELEMENT(#7427,-3.);
#4141=DERIVED_UNIT_ELEMENT(#4163,1.);
#4142=DERIVED_UNIT_ELEMENT(#7427,-3.);
#4143=DERIVED_UNIT_ELEMENT(#4163,1.);
#4144=DERIVED_UNIT_ELEMENT(#7427,-3.);
#4145=DERIVED_UNIT_ELEMENT(#4163,1.);
#4146=DERIVED_UNIT_ELEMENT(#7427,-3.);
#4147=DERIVED_UNIT_ELEMENT(#4163,1.);
#4148=DERIVED_UNIT_ELEMENT(#7427,-3.);
#4149=DERIVED_UNIT_ELEMENT(#4163,1.);
#4150=DERIVED_UNIT_ELEMENT(#7427,-3.);
#4151=DERIVED_UNIT_ELEMENT(#4163,1.);
#4152=DERIVED_UNIT_ELEMENT(#7427,-3.);
#4153=DERIVED_UNIT_ELEMENT(#4163,1.);
#4154=DERIVED_UNIT_ELEMENT(#7427,-3.);
#4155=DERIVED_UNIT_ELEMENT(#4163,1.);
#4156=DERIVED_UNIT_ELEMENT(#7427,-3.);
#4157=DERIVED_UNIT_ELEMENT(#4163,1.);
#4158=DERIVED_UNIT_ELEMENT(#7427,-3.);
#4159=DERIVED_UNIT_ELEMENT(#4163,1.);
#4160=DERIVED_UNIT_ELEMENT(#7427,-3.);
#4161=DERIVED_UNIT_ELEMENT(#4163,1.);
#4162=DERIVED_UNIT_ELEMENT(#7427,-3.);
#4163=(
MASS_UNIT()
NAMED_UNIT(*)
SI_UNIT(.KILO.,.GRAM.)
);
#4164=DERIVED_UNIT((#4111,#4112));
#4165=DERIVED_UNIT((#4113,#4114));
#4166=DERIVED_UNIT((#4115,#4116));
#4167=DERIVED_UNIT((#4117,#4118));
#4168=DERIVED_UNIT((#4119,#4120));
#4169=DERIVED_UNIT((#4121,#4122));
#4170=DERIVED_UNIT((#4123,#4124));
#4171=DERIVED_UNIT((#4125,#4126));
#4172=DERIVED_UNIT((#4127,#4128));
#4173=DERIVED_UNIT((#4129,#4130));
#4174=DERIVED_UNIT((#4131,#4132));
#4175=DERIVED_UNIT((#4133,#4134));
#4176=DERIVED_UNIT((#4135,#4136));
#4177=DERIVED_UNIT((#4137,#4138));
#4178=DERIVED_UNIT((#4139,#4140));
#4179=DERIVED_UNIT((#4141,#4142));
#4180=DERIVED_UNIT((#4143,#4144));
#4181=DERIVED_UNIT((#4145,#4146));
#4182=DERIVED_UNIT((#4147,#4148));
#4183=DERIVED_UNIT((#4149,#4150));
#4184=DERIVED_UNIT((#4151,#4152));
#4185=DERIVED_UNIT((#4153,#4154));
#4186=DERIVED_UNIT((#4155,#4156));
#4187=DERIVED_UNIT((#4157,#4158));
#4188=DERIVED_UNIT((#4159,#4160));
#4189=DERIVED_UNIT((#4161,#4162));
#4190=MEASURE_REPRESENTATION_ITEM('density measure',
POSITIVE_RATIO_MEASURE(7850.),#4164);
#4191=MEASURE_REPRESENTATION_ITEM('density measure',
POSITIVE_RATIO_MEASURE(7850.),#4165);
#4192=MEASURE_REPRESENTATION_ITEM('density measure',
POSITIVE_RATIO_MEASURE(7850.),#4166);
#4193=MEASURE_REPRESENTATION_ITEM('density measure',
POSITIVE_RATIO_MEASURE(7850.),#4167);
#4194=MEASURE_REPRESENTATION_ITEM('density measure',
POSITIVE_RATIO_MEASURE(7850.),#4168);
#4195=MEASURE_REPRESENTATION_ITEM('density measure',
POSITIVE_RATIO_MEASURE(7850.),#4169);
#4196=MEASURE_REPRESENTATION_ITEM('density measure',
POSITIVE_RATIO_MEASURE(7850.),#4170);
#4197=MEASURE_REPRESENTATION_ITEM('density measure',
POSITIVE_RATIO_MEASURE(7850.),#4171);
#4198=MEASURE_REPRESENTATION_ITEM('density measure',
POSITIVE_RATIO_MEASURE(7850.),#4172);
#4199=MEASURE_REPRESENTATION_ITEM('density measure',
POSITIVE_RATIO_MEASURE(7850.),#4173);
#4200=MEASURE_REPRESENTATION_ITEM('density measure',
POSITIVE_RATIO_MEASURE(7850.),#4174);
#4201=MEASURE_REPRESENTATION_ITEM('density measure',
POSITIVE_RATIO_MEASURE(7850.),#4175);
#4202=MEASURE_REPRESENTATION_ITEM('density measure',
POSITIVE_RATIO_MEASURE(7850.),#4176);
#4203=MEASURE_REPRESENTATION_ITEM('density measure',
POSITIVE_RATIO_MEASURE(7850.),#4177);
#4204=MEASURE_REPRESENTATION_ITEM('density measure',
POSITIVE_RATIO_MEASURE(7850.),#4178);
#4205=MEASURE_REPRESENTATION_ITEM('density measure',
POSITIVE_RATIO_MEASURE(7850.),#4179);
#4206=MEASURE_REPRESENTATION_ITEM('density measure',
POSITIVE_RATIO_MEASURE(7850.),#4180);
#4207=MEASURE_REPRESENTATION_ITEM('density measure',
POSITIVE_RATIO_MEASURE(7850.),#4181);
#4208=MEASURE_REPRESENTATION_ITEM('density measure',
POSITIVE_RATIO_MEASURE(7850.),#4182);
#4209=MEASURE_REPRESENTATION_ITEM('density measure',
POSITIVE_RATIO_MEASURE(7850.),#4183);
#4210=MEASURE_REPRESENTATION_ITEM('density measure',
POSITIVE_RATIO_MEASURE(7850.),#4184);
#4211=MEASURE_REPRESENTATION_ITEM('density measure',
POSITIVE_RATIO_MEASURE(7850.),#4185);
#4212=MEASURE_REPRESENTATION_ITEM('density measure',
POSITIVE_RATIO_MEASURE(7850.),#4186);
#4213=MEASURE_REPRESENTATION_ITEM('density measure',
POSITIVE_RATIO_MEASURE(7850.),#4187);
#4214=MEASURE_REPRESENTATION_ITEM('density measure',
POSITIVE_RATIO_MEASURE(7850.),#4188);
#4215=MEASURE_REPRESENTATION_ITEM('density measure',
POSITIVE_RATIO_MEASURE(7850.),#4189);
#4216=PROPERTY_DEFINITION_REPRESENTATION(#4346,#4268);
#4217=PROPERTY_DEFINITION_REPRESENTATION(#4347,#4269);
#4218=PROPERTY_DEFINITION_REPRESENTATION(#4348,#4270);
#4219=PROPERTY_DEFINITION_REPRESENTATION(#4349,#4271);
#4220=PROPERTY_DEFINITION_REPRESENTATION(#4350,#4272);
#4221=PROPERTY_DEFINITION_REPRESENTATION(#4351,#4273);
#4222=PROPERTY_DEFINITION_REPRESENTATION(#4352,#4274);
#4223=PROPERTY_DEFINITION_REPRESENTATION(#4353,#4275);
#4224=PROPERTY_DEFINITION_REPRESENTATION(#4354,#4276);
#4225=PROPERTY_DEFINITION_REPRESENTATION(#4355,#4277);
#4226=PROPERTY_DEFINITION_REPRESENTATION(#4356,#4278);
#4227=PROPERTY_DEFINITION_REPRESENTATION(#4357,#4279);
#4228=PROPERTY_DEFINITION_REPRESENTATION(#4358,#4280);
#4229=PROPERTY_DEFINITION_REPRESENTATION(#4359,#4281);
#4230=PROPERTY_DEFINITION_REPRESENTATION(#4360,#4282);
#4231=PROPERTY_DEFINITION_REPRESENTATION(#4361,#4283);
#4232=PROPERTY_DEFINITION_REPRESENTATION(#4362,#4284);
#4233=PROPERTY_DEFINITION_REPRESENTATION(#4363,#4285);
#4234=PROPERTY_DEFINITION_REPRESENTATION(#4364,#4286);
#4235=PROPERTY_DEFINITION_REPRESENTATION(#4365,#4287);
#4236=PROPERTY_DEFINITION_REPRESENTATION(#4366,#4288);
#4237=PROPERTY_DEFINITION_REPRESENTATION(#4367,#4289);
#4238=PROPERTY_DEFINITION_REPRESENTATION(#4368,#4290);
#4239=PROPERTY_DEFINITION_REPRESENTATION(#4369,#4291);
#4240=PROPERTY_DEFINITION_REPRESENTATION(#4370,#4292);
#4241=PROPERTY_DEFINITION_REPRESENTATION(#4371,#4293);
#4242=PROPERTY_DEFINITION_REPRESENTATION(#4372,#4294);
#4243=PROPERTY_DEFINITION_REPRESENTATION(#4373,#4295);
#4244=PROPERTY_DEFINITION_REPRESENTATION(#4374,#4296);
#4245=PROPERTY_DEFINITION_REPRESENTATION(#4375,#4297);
#4246=PROPERTY_DEFINITION_REPRESENTATION(#4376,#4298);
#4247=PROPERTY_DEFINITION_REPRESENTATION(#4377,#4299);
#4248=PROPERTY_DEFINITION_REPRESENTATION(#4378,#4300);
#4249=PROPERTY_DEFINITION_REPRESENTATION(#4379,#4301);
#4250=PROPERTY_DEFINITION_REPRESENTATION(#4380,#4302);
#4251=PROPERTY_DEFINITION_REPRESENTATION(#4381,#4303);
#4252=PROPERTY_DEFINITION_REPRESENTATION(#4382,#4304);
#4253=PROPERTY_DEFINITION_REPRESENTATION(#4383,#4305);
#4254=PROPERTY_DEFINITION_REPRESENTATION(#4384,#4306);
#4255=PROPERTY_DEFINITION_REPRESENTATION(#4385,#4307);
#4256=PROPERTY_DEFINITION_REPRESENTATION(#4386,#4308);
#4257=PROPERTY_DEFINITION_REPRESENTATION(#4387,#4309);
#4258=PROPERTY_DEFINITION_REPRESENTATION(#4388,#4310);
#4259=PROPERTY_DEFINITION_REPRESENTATION(#4389,#4311);
#4260=PROPERTY_DEFINITION_REPRESENTATION(#4390,#4312);
#4261=PROPERTY_DEFINITION_REPRESENTATION(#4391,#4313);
#4262=PROPERTY_DEFINITION_REPRESENTATION(#4392,#4314);
#4263=PROPERTY_DEFINITION_REPRESENTATION(#4393,#4315);
#4264=PROPERTY_DEFINITION_REPRESENTATION(#4394,#4316);
#4265=PROPERTY_DEFINITION_REPRESENTATION(#4395,#4317);
#4266=PROPERTY_DEFINITION_REPRESENTATION(#4396,#4318);
#4267=PROPERTY_DEFINITION_REPRESENTATION(#4397,#4319);
#4268=REPRESENTATION('material name',(#4320),#7398);
#4269=REPRESENTATION('density',(#4190),#7398);
#4270=REPRESENTATION('material name',(#4321),#7399);
#4271=REPRESENTATION('density',(#4191),#7399);
#4272=REPRESENTATION('material name',(#4322),#7400);
#4273=REPRESENTATION('density',(#4192),#7400);
#4274=REPRESENTATION('material name',(#4323),#7401);
#4275=REPRESENTATION('density',(#4193),#7401);
#4276=REPRESENTATION('material name',(#4324),#7402);
#4277=REPRESENTATION('density',(#4194),#7402);
#4278=REPRESENTATION('material name',(#4325),#7403);
#4279=REPRESENTATION('density',(#4195),#7403);
#4280=REPRESENTATION('material name',(#4326),#7404);
#4281=REPRESENTATION('density',(#4196),#7404);
#4282=REPRESENTATION('material name',(#4327),#7405);
#4283=REPRESENTATION('density',(#4197),#7405);
#4284=REPRESENTATION('material name',(#4328),#7406);
#4285=REPRESENTATION('density',(#4198),#7406);
#4286=REPRESENTATION('material name',(#4329),#7407);
#4287=REPRESENTATION('density',(#4199),#7407);
#4288=REPRESENTATION('material name',(#4330),#7408);
#4289=REPRESENTATION('density',(#4200),#7408);
#4290=REPRESENTATION('material name',(#4331),#7409);
#4291=REPRESENTATION('density',(#4201),#7409);
#4292=REPRESENTATION('material name',(#4332),#7410);
#4293=REPRESENTATION('density',(#4202),#7410);
#4294=REPRESENTATION('material name',(#4333),#7411);
#4295=REPRESENTATION('density',(#4203),#7411);
#4296=REPRESENTATION('material name',(#4334),#7412);
#4297=REPRESENTATION('density',(#4204),#7412);
#4298=REPRESENTATION('material name',(#4335),#7413);
#4299=REPRESENTATION('density',(#4205),#7413);
#4300=REPRESENTATION('material name',(#4336),#7414);
#4301=REPRESENTATION('density',(#4206),#7414);
#4302=REPRESENTATION('material name',(#4337),#7415);
#4303=REPRESENTATION('density',(#4207),#7415);
#4304=REPRESENTATION('material name',(#4338),#7416);
#4305=REPRESENTATION('density',(#4208),#7416);
#4306=REPRESENTATION('material name',(#4339),#7417);
#4307=REPRESENTATION('density',(#4209),#7417);
#4308=REPRESENTATION('material name',(#4340),#7419);
#4309=REPRESENTATION('density',(#4210),#7419);
#4310=REPRESENTATION('material name',(#4341),#7420);
#4311=REPRESENTATION('density',(#4211),#7420);
#4312=REPRESENTATION('material name',(#4342),#7421);
#4313=REPRESENTATION('density',(#4212),#7421);
#4314=REPRESENTATION('material name',(#4343),#7422);
#4315=REPRESENTATION('density',(#4213),#7422);
#4316=REPRESENTATION('material name',(#4344),#7423);
#4317=REPRESENTATION('density',(#4214),#7423);
#4318=REPRESENTATION('material name',(#4345),#7424);
#4319=REPRESENTATION('density',(#4215),#7424);
#4320=DESCRIPTIVE_REPRESENTATION_ITEM('Steel','Steel');
#4321=DESCRIPTIVE_REPRESENTATION_ITEM('Steel','Steel');
#4322=DESCRIPTIVE_REPRESENTATION_ITEM('Steel','Steel');
#4323=DESCRIPTIVE_REPRESENTATION_ITEM('Steel','Steel');
#4324=DESCRIPTIVE_REPRESENTATION_ITEM('Steel','Steel');
#4325=DESCRIPTIVE_REPRESENTATION_ITEM('Steel','Steel');
#4326=DESCRIPTIVE_REPRESENTATION_ITEM('Steel','Steel');
#4327=DESCRIPTIVE_REPRESENTATION_ITEM('Steel','Steel');
#4328=DESCRIPTIVE_REPRESENTATION_ITEM('Steel','Steel');
#4329=DESCRIPTIVE_REPRESENTATION_ITEM('Steel','Steel');
#4330=DESCRIPTIVE_REPRESENTATION_ITEM('Steel','Steel');
#4331=DESCRIPTIVE_REPRESENTATION_ITEM('Steel','Steel');
#4332=DESCRIPTIVE_REPRESENTATION_ITEM('Steel','Steel');
#4333=DESCRIPTIVE_REPRESENTATION_ITEM('Steel','Steel');
#4334=DESCRIPTIVE_REPRESENTATION_ITEM('Steel','Steel');
#4335=DESCRIPTIVE_REPRESENTATION_ITEM('Steel','Steel');
#4336=DESCRIPTIVE_REPRESENTATION_ITEM('Steel','Steel');
#4337=DESCRIPTIVE_REPRESENTATION_ITEM('Steel','Steel');
#4338=DESCRIPTIVE_REPRESENTATION_ITEM('Steel','Steel');
#4339=DESCRIPTIVE_REPRESENTATION_ITEM('Steel','Steel');
#4340=DESCRIPTIVE_REPRESENTATION_ITEM('Steel','Steel');
#4341=DESCRIPTIVE_REPRESENTATION_ITEM('Steel','Steel');
#4342=DESCRIPTIVE_REPRESENTATION_ITEM('Steel','Steel');
#4343=DESCRIPTIVE_REPRESENTATION_ITEM('Steel','Steel');
#4344=DESCRIPTIVE_REPRESENTATION_ITEM('Steel','Steel');
#4345=DESCRIPTIVE_REPRESENTATION_ITEM('Steel','Steel');
#4346=PROPERTY_DEFINITION('material property','material name',#7565);
#4347=PROPERTY_DEFINITION('material property','density of part',#7565);
#4348=PROPERTY_DEFINITION('material property','material name',#7566);
#4349=PROPERTY_DEFINITION('material property','density of part',#7566);
#4350=PROPERTY_DEFINITION('material property','material name',#7567);
#4351=PROPERTY_DEFINITION('material property','density of part',#7567);
#4352=PROPERTY_DEFINITION('material property','material name',#7568);
#4353=PROPERTY_DEFINITION('material property','density of part',#7568);
#4354=PROPERTY_DEFINITION('material property','material name',#7569);
#4355=PROPERTY_DEFINITION('material property','density of part',#7569);
#4356=PROPERTY_DEFINITION('material property','material name',#7570);
#4357=PROPERTY_DEFINITION('material property','density of part',#7570);
#4358=PROPERTY_DEFINITION('material property','material name',#7571);
#4359=PROPERTY_DEFINITION('material property','density of part',#7571);
#4360=PROPERTY_DEFINITION('material property','material name',#7572);
#4361=PROPERTY_DEFINITION('material property','density of part',#7572);
#4362=PROPERTY_DEFINITION('material property','material name',#7573);
#4363=PROPERTY_DEFINITION('material property','density of part',#7573);
#4364=PROPERTY_DEFINITION('material property','material name',#7574);
#4365=PROPERTY_DEFINITION('material property','density of part',#7574);
#4366=PROPERTY_DEFINITION('material property','material name',#7575);
#4367=PROPERTY_DEFINITION('material property','density of part',#7575);
#4368=PROPERTY_DEFINITION('material property','material name',#7576);
#4369=PROPERTY_DEFINITION('material property','density of part',#7576);
#4370=PROPERTY_DEFINITION('material property','material name',#7577);
#4371=PROPERTY_DEFINITION('material property','density of part',#7577);
#4372=PROPERTY_DEFINITION('material property','material name',#7578);
#4373=PROPERTY_DEFINITION('material property','density of part',#7578);
#4374=PROPERTY_DEFINITION('material property','material name',#7579);
#4375=PROPERTY_DEFINITION('material property','density of part',#7579);
#4376=PROPERTY_DEFINITION('material property','material name',#7580);
#4377=PROPERTY_DEFINITION('material property','density of part',#7580);
#4378=PROPERTY_DEFINITION('material property','material name',#7581);
#4379=PROPERTY_DEFINITION('material property','density of part',#7581);
#4380=PROPERTY_DEFINITION('material property','material name',#7582);
#4381=PROPERTY_DEFINITION('material property','density of part',#7582);
#4382=PROPERTY_DEFINITION('material property','material name',#7583);
#4383=PROPERTY_DEFINITION('material property','density of part',#7583);
#4384=PROPERTY_DEFINITION('material property','material name',#7584);
#4385=PROPERTY_DEFINITION('material property','density of part',#7584);
#4386=PROPERTY_DEFINITION('material property','material name',#7586);
#4387=PROPERTY_DEFINITION('material property','density of part',#7586);
#4388=PROPERTY_DEFINITION('material property','material name',#7587);
#4389=PROPERTY_DEFINITION('material property','density of part',#7587);
#4390=PROPERTY_DEFINITION('material property','material name',#7588);
#4391=PROPERTY_DEFINITION('material property','density of part',#7588);
#4392=PROPERTY_DEFINITION('material property','material name',#7589);
#4393=PROPERTY_DEFINITION('material property','density of part',#7589);
#4394=PROPERTY_DEFINITION('material property','material name',#7590);
#4395=PROPERTY_DEFINITION('material property','density of part',#7590);
#4396=PROPERTY_DEFINITION('material property','material name',#7591);
#4397=PROPERTY_DEFINITION('material property','density of part',#7591);
#4398=AXIS2_PLACEMENT_3D('',#6200,#4896,#4897);
#4399=AXIS2_PLACEMENT_3D('',#6201,#4898,#4899);
#4400=AXIS2_PLACEMENT_3D('',#6202,#4900,#4901);
#4401=AXIS2_PLACEMENT_3D('',#6203,#4902,#4903);
#4402=AXIS2_PLACEMENT_3D('',#6205,#4904,#4905);
#4403=AXIS2_PLACEMENT_3D('',#6208,#4907,#4908);
#4404=AXIS2_PLACEMENT_3D('',#6209,#4909,#4910);
#4405=AXIS2_PLACEMENT_3D('',#6210,#4911,#4912);
#4406=AXIS2_PLACEMENT_3D('',#6212,#4913,#4914);
#4407=AXIS2_PLACEMENT_3D('',#6215,#4916,#4917);
#4408=AXIS2_PLACEMENT_3D('',#6216,#4918,#4919);
#4409=AXIS2_PLACEMENT_3D('',#6217,#4920,#4921);
#4410=AXIS2_PLACEMENT_3D('',#6219,#4922,#4923);
#4411=AXIS2_PLACEMENT_3D('',#6222,#4925,#4926);
#4412=AXIS2_PLACEMENT_3D('',#6223,#4927,#4928);
#4413=AXIS2_PLACEMENT_3D('',#6225,#4929,#4930);
#4414=AXIS2_PLACEMENT_3D('',#6228,#4932,#4933);
#4415=AXIS2_PLACEMENT_3D('',#6229,#4934,#4935);
#4416=AXIS2_PLACEMENT_3D('',#6231,#4936,#4937);
#4417=AXIS2_PLACEMENT_3D('',#6234,#4939,#4940);
#4418=AXIS2_PLACEMENT_3D('',#6235,#4941,#4942);
#4419=AXIS2_PLACEMENT_3D('',#6237,#4943,#4944);
#4420=AXIS2_PLACEMENT_3D('',#6240,#4946,#4947);
#4421=AXIS2_PLACEMENT_3D('',#6241,#4948,#4949);
#4422=AXIS2_PLACEMENT_3D('',#6246,#4951,#4952);
#4423=AXIS2_PLACEMENT_3D('',#6249,#4954,#4955);
#4424=AXIS2_PLACEMENT_3D('',#6250,#4956,#4957);
#4425=AXIS2_PLACEMENT_3D('',#6254,#4959,#4960);
#4426=AXIS2_PLACEMENT_3D('',#6256,#4962,#4963);
#4427=AXIS2_PLACEMENT_3D('',#6266,#4969,#4970);
#4428=AXIS2_PLACEMENT_3D('',#6268,#4971,#4972);
#4429=AXIS2_PLACEMENT_3D('',#6271,#4974,#4975);
#4430=AXIS2_PLACEMENT_3D('',#6272,#4976,#4977);
#4431=AXIS2_PLACEMENT_3D('',#6274,#4978,#4979);
#4432=AXIS2_PLACEMENT_3D('',#6277,#4981,#4982);
#4433=AXIS2_PLACEMENT_3D('',#6278,#4983,#4984);
#4434=AXIS2_PLACEMENT_3D('',#6280,#4985,#4986);
#4435=AXIS2_PLACEMENT_3D('',#6281,#4987,#4988);
#4436=AXIS2_PLACEMENT_3D('',#6282,#4989,#4990);
#4437=AXIS2_PLACEMENT_3D('',#6283,#4991,#4992);
#4438=AXIS2_PLACEMENT_3D('',#6284,#4993,#4994);
#4439=AXIS2_PLACEMENT_3D('',#6290,#4998,#4999);
#4440=AXIS2_PLACEMENT_3D('',#6294,#5002,#5003);
#4441=AXIS2_PLACEMENT_3D('',#6298,#5006,#5007);
#4442=AXIS2_PLACEMENT_3D('',#6300,#5009,#5010);
#4443=AXIS2_PLACEMENT_3D('',#6301,#5011,#5012);
#4444=AXIS2_PLACEMENT_3D('',#6302,#5013,#5014);
#4445=AXIS2_PLACEMENT_3D('',#6304,#5015,#5016);
#4446=AXIS2_PLACEMENT_3D('',#6306,#5017,#5018);
#4447=AXIS2_PLACEMENT_3D('',#6307,#5019,#5020);
#4448=AXIS2_PLACEMENT_3D('',#6310,#5022,#5023);
#4449=AXIS2_PLACEMENT_3D('',#6311,#5024,#5025);
#4450=AXIS2_PLACEMENT_3D('',#6313,#5026,#5027);
#4451=AXIS2_PLACEMENT_3D('',#6316,#5029,#5030);
#4452=AXIS2_PLACEMENT_3D('',#6317,#5031,#5032);
#4453=AXIS2_PLACEMENT_3D('',#6318,#5033,#5034);
#4454=AXIS2_PLACEMENT_3D('',#6319,#5035,#5036);
#4455=AXIS2_PLACEMENT_3D('',#6320,#5037,#5038);
#4456=AXIS2_PLACEMENT_3D('',#6322,#5039,#5040);
#4457=AXIS2_PLACEMENT_3D('',#6325,#5042,#5043);
#4458=AXIS2_PLACEMENT_3D('',#6326,#5044,#5045);
#4459=AXIS2_PLACEMENT_3D('',#6327,#5046,#5047);
#4460=AXIS2_PLACEMENT_3D('',#6329,#5048,#5049);
#4461=AXIS2_PLACEMENT_3D('',#6332,#5051,#5052);
#4462=AXIS2_PLACEMENT_3D('',#6333,#5053,#5054);
#4463=AXIS2_PLACEMENT_3D('',#6334,#5055,#5056);
#4464=AXIS2_PLACEMENT_3D('',#6336,#5057,#5058);
#4465=AXIS2_PLACEMENT_3D('',#6339,#5060,#5061);
#4466=AXIS2_PLACEMENT_3D('',#6340,#5062,#5063);
#4467=AXIS2_PLACEMENT_3D('',#6342,#5064,#5065);
#4468=AXIS2_PLACEMENT_3D('',#6345,#5067,#5068);
#4469=AXIS2_PLACEMENT_3D('',#6346,#5069,#5070);
#4470=AXIS2_PLACEMENT_3D('',#6348,#5071,#5072);
#4471=AXIS2_PLACEMENT_3D('',#6351,#5074,#5075);
#4472=AXIS2_PLACEMENT_3D('',#6352,#5076,#5077);
#4473=AXIS2_PLACEMENT_3D('',#6354,#5078,#5079);
#4474=AXIS2_PLACEMENT_3D('',#6357,#5081,#5082);
#4475=AXIS2_PLACEMENT_3D('',#6358,#5083,#5084);
#4476=AXIS2_PLACEMENT_3D('',#6363,#5086,#5087);
#4477=AXIS2_PLACEMENT_3D('',#6366,#5089,#5090);
#4478=AXIS2_PLACEMENT_3D('',#6367,#5091,#5092);
#4479=AXIS2_PLACEMENT_3D('',#6371,#5094,#5095);
#4480=AXIS2_PLACEMENT_3D('',#6373,#5097,#5098);
#4481=AXIS2_PLACEMENT_3D('',#6383,#5104,#5105);
#4482=AXIS2_PLACEMENT_3D('',#6385,#5106,#5107);
#4483=AXIS2_PLACEMENT_3D('',#6388,#5109,#5110);
#4484=AXIS2_PLACEMENT_3D('',#6389,#5111,#5112);
#4485=AXIS2_PLACEMENT_3D('',#6391,#5113,#5114);
#4486=AXIS2_PLACEMENT_3D('',#6394,#5116,#5117);
#4487=AXIS2_PLACEMENT_3D('',#6395,#5118,#5119);
#4488=AXIS2_PLACEMENT_3D('',#6396,#5120,#5121);
#4489=AXIS2_PLACEMENT_3D('',#6398,#5122,#5123);
#4490=AXIS2_PLACEMENT_3D('',#6399,#5124,#5125);
#4491=AXIS2_PLACEMENT_3D('',#6400,#5126,#5127);
#4492=AXIS2_PLACEMENT_3D('',#6401,#5128,#5129);
#4493=AXIS2_PLACEMENT_3D('',#6407,#5133,#5134);
#4494=AXIS2_PLACEMENT_3D('',#6411,#5137,#5138);
#4495=AXIS2_PLACEMENT_3D('',#6415,#5141,#5142);
#4496=AXIS2_PLACEMENT_3D('',#6417,#5144,#5145);
#4497=AXIS2_PLACEMENT_3D('',#6418,#5146,#5147);
#4498=AXIS2_PLACEMENT_3D('',#6419,#5148,#5149);
#4499=AXIS2_PLACEMENT_3D('',#6421,#5150,#5151);
#4500=AXIS2_PLACEMENT_3D('',#6423,#5152,#5153);
#4501=AXIS2_PLACEMENT_3D('',#6424,#5154,#5155);
#4502=AXIS2_PLACEMENT_3D('',#6426,#5156,#5157);
#4503=AXIS2_PLACEMENT_3D('',#6428,#5159,#5160);
#4504=AXIS2_PLACEMENT_3D('',#6430,#5161,#5162);
#4505=AXIS2_PLACEMENT_3D('',#6433,#5164,#5165);
#4506=AXIS2_PLACEMENT_3D('',#6434,#5166,#5167);
#4507=AXIS2_PLACEMENT_3D('',#6435,#5168,#5169);
#4508=AXIS2_PLACEMENT_3D('',#6436,#5170,#5171);
#4509=AXIS2_PLACEMENT_3D('',#6437,#5172,#5173);
#4510=AXIS2_PLACEMENT_3D('',#6439,#5174,#5175);
#4511=AXIS2_PLACEMENT_3D('',#6442,#5177,#5178);
#4512=AXIS2_PLACEMENT_3D('',#6443,#5179,#5180);
#4513=AXIS2_PLACEMENT_3D('',#6445,#5181,#5182);
#4514=AXIS2_PLACEMENT_3D('',#6448,#5184,#5185);
#4515=AXIS2_PLACEMENT_3D('',#6449,#5186,#5187);
#4516=AXIS2_PLACEMENT_3D('',#6451,#5188,#5189);
#4517=AXIS2_PLACEMENT_3D('',#6454,#5191,#5192);
#4518=AXIS2_PLACEMENT_3D('',#6455,#5193,#5194);
#4519=AXIS2_PLACEMENT_3D('',#6457,#5195,#5196);
#4520=AXIS2_PLACEMENT_3D('',#6460,#5198,#5199);
#4521=AXIS2_PLACEMENT_3D('',#6461,#5200,#5201);
#4522=AXIS2_PLACEMENT_3D('',#6470,#5206,#5207);
#4523=AXIS2_PLACEMENT_3D('',#6479,#5212,#5213);
#4524=AXIS2_PLACEMENT_3D('',#6485,#5217,#5218);
#4525=AXIS2_PLACEMENT_3D('',#6491,#5222,#5223);
#4526=AXIS2_PLACEMENT_3D('',#6492,#5224,#5225);
#4527=AXIS2_PLACEMENT_3D('',#6502,#5231,#5232);
#4528=AXIS2_PLACEMENT_3D('',#6506,#5235,#5236);
#4529=AXIS2_PLACEMENT_3D('',#6510,#5239,#5240);
#4530=AXIS2_PLACEMENT_3D('',#6511,#5241,#5242);
#4531=AXIS2_PLACEMENT_3D('',#6512,#5243,#5244);
#4532=AXIS2_PLACEMENT_3D('',#6516,#5247,#5248);
#4533=AXIS2_PLACEMENT_3D('',#6520,#5251,#5252);
#4534=AXIS2_PLACEMENT_3D('',#6522,#5254,#5255);
#4535=AXIS2_PLACEMENT_3D('',#6523,#5256,#5257);
#4536=AXIS2_PLACEMENT_3D('',#6524,#5258,#5259);
#4537=AXIS2_PLACEMENT_3D('',#6526,#5260,#5261);
#4538=AXIS2_PLACEMENT_3D('',#6528,#5262,#5263);
#4539=AXIS2_PLACEMENT_3D('',#6529,#5264,#5265);
#4540=AXIS2_PLACEMENT_3D('',#6531,#5266,#5267);
#4541=AXIS2_PLACEMENT_3D('',#6533,#5269,#5270);
#4542=AXIS2_PLACEMENT_3D('',#6535,#5271,#5272);
#4543=AXIS2_PLACEMENT_3D('',#6536,#5273,#5274);
#4544=AXIS2_PLACEMENT_3D('',#6539,#5276,#5277);
#4545=AXIS2_PLACEMENT_3D('',#6540,#5278,#5279);
#4546=AXIS2_PLACEMENT_3D('',#6543,#5281,#5282);
#4547=AXIS2_PLACEMENT_3D('',#6544,#5283,#5284);
#4548=AXIS2_PLACEMENT_3D('',#6545,#5285,#5286);
#4549=AXIS2_PLACEMENT_3D('',#6546,#5287,#5288);
#4550=AXIS2_PLACEMENT_3D('',#6548,#5289,#5290);
#4551=AXIS2_PLACEMENT_3D('',#6549,#5291,#5292);
#4552=AXIS2_PLACEMENT_3D('',#6550,#5293,#5294);
#4553=AXIS2_PLACEMENT_3D('',#6551,#5295,#5296);
#4554=AXIS2_PLACEMENT_3D('',#6553,#5297,#5298);
#4555=AXIS2_PLACEMENT_3D('',#6556,#5300,#5301);
#4556=AXIS2_PLACEMENT_3D('',#6557,#5302,#5303);
#4557=AXIS2_PLACEMENT_3D('',#6559,#5304,#5305);
#4558=AXIS2_PLACEMENT_3D('',#6560,#5306,#5307);
#4559=AXIS2_PLACEMENT_3D('',#6562,#5308,#5309);
#4560=AXIS2_PLACEMENT_3D('',#6564,#5311,#5312);
#4561=AXIS2_PLACEMENT_3D('',#6566,#5313,#5314);
#4562=AXIS2_PLACEMENT_3D('',#6569,#5316,#5317);
#4563=AXIS2_PLACEMENT_3D('',#6570,#5318,#5319);
#4564=AXIS2_PLACEMENT_3D('',#6571,#5320,#5321);
#4565=AXIS2_PLACEMENT_3D('',#6572,#5322,#5323);
#4566=AXIS2_PLACEMENT_3D('',#6573,#5324,#5325);
#4567=AXIS2_PLACEMENT_3D('',#6575,#5326,#5327);
#4568=AXIS2_PLACEMENT_3D('',#6578,#5329,#5330);
#4569=AXIS2_PLACEMENT_3D('',#6579,#5331,#5332);
#4570=AXIS2_PLACEMENT_3D('',#6580,#5333,#5334);
#4571=AXIS2_PLACEMENT_3D('',#6582,#5335,#5336);
#4572=AXIS2_PLACEMENT_3D('',#6585,#5338,#5339);
#4573=AXIS2_PLACEMENT_3D('',#6586,#5340,#5341);
#4574=AXIS2_PLACEMENT_3D('',#6587,#5342,#5343);
#4575=AXIS2_PLACEMENT_3D('',#6589,#5344,#5345);
#4576=AXIS2_PLACEMENT_3D('',#6592,#5347,#5348);
#4577=AXIS2_PLACEMENT_3D('',#6593,#5349,#5350);
#4578=AXIS2_PLACEMENT_3D('',#6595,#5351,#5352);
#4579=AXIS2_PLACEMENT_3D('',#6598,#5354,#5355);
#4580=AXIS2_PLACEMENT_3D('',#6599,#5356,#5357);
#4581=AXIS2_PLACEMENT_3D('',#6601,#5358,#5359);
#4582=AXIS2_PLACEMENT_3D('',#6604,#5361,#5362);
#4583=AXIS2_PLACEMENT_3D('',#6605,#5363,#5364);
#4584=AXIS2_PLACEMENT_3D('',#6607,#5365,#5366);
#4585=AXIS2_PLACEMENT_3D('',#6610,#5368,#5369);
#4586=AXIS2_PLACEMENT_3D('',#6611,#5370,#5371);
#4587=AXIS2_PLACEMENT_3D('',#6613,#5372,#5373);
#4588=AXIS2_PLACEMENT_3D('',#6616,#5375,#5376);
#4589=AXIS2_PLACEMENT_3D('',#6617,#5377,#5378);
#4590=AXIS2_PLACEMENT_3D('',#6626,#5383,#5384);
#4591=AXIS2_PLACEMENT_3D('',#6632,#5388,#5389);
#4592=AXIS2_PLACEMENT_3D('',#6638,#5393,#5394);
#4593=AXIS2_PLACEMENT_3D('',#6641,#5397,#5398);
#4594=AXIS2_PLACEMENT_3D('',#6642,#5399,#5400);
#4595=AXIS2_PLACEMENT_3D('',#6643,#5401,#5402);
#4596=AXIS2_PLACEMENT_3D('',#6644,#5403,#5404);
#4597=AXIS2_PLACEMENT_3D('',#6646,#5405,#5406);
#4598=AXIS2_PLACEMENT_3D('',#6649,#5408,#5409);
#4599=AXIS2_PLACEMENT_3D('',#6650,#5410,#5411);
#4600=AXIS2_PLACEMENT_3D('',#6652,#5412,#5413);
#4601=AXIS2_PLACEMENT_3D('',#6655,#5415,#5416);
#4602=AXIS2_PLACEMENT_3D('',#6656,#5417,#5418);
#4603=AXIS2_PLACEMENT_3D('',#6657,#5419,#5420);
#4604=AXIS2_PLACEMENT_3D('',#6658,#5421,#5422);
#4605=AXIS2_PLACEMENT_3D('',#6659,#5423,#5424);
#4606=AXIS2_PLACEMENT_3D('',#6661,#5425,#5426);
#4607=AXIS2_PLACEMENT_3D('',#6664,#5428,#5429);
#4608=AXIS2_PLACEMENT_3D('',#6665,#5430,#5431);
#4609=AXIS2_PLACEMENT_3D('',#6667,#5432,#5433);
#4610=AXIS2_PLACEMENT_3D('',#6670,#5435,#5436);
#4611=AXIS2_PLACEMENT_3D('',#6671,#5437,#5438);
#4612=AXIS2_PLACEMENT_3D('',#6672,#5439,#5440);
#4613=AXIS2_PLACEMENT_3D('',#6673,#5441,#5442);
#4614=AXIS2_PLACEMENT_3D('',#6674,#5443,#5444);
#4615=AXIS2_PLACEMENT_3D('',#6676,#5445,#5446);
#4616=AXIS2_PLACEMENT_3D('',#6679,#5448,#5449);
#4617=AXIS2_PLACEMENT_3D('',#6680,#5450,#5451);
#4618=AXIS2_PLACEMENT_3D('',#6682,#5452,#5453);
#4619=AXIS2_PLACEMENT_3D('',#6685,#5455,#5456);
#4620=AXIS2_PLACEMENT_3D('',#6686,#5457,#5458);
#4621=AXIS2_PLACEMENT_3D('',#6687,#5459,#5460);
#4622=AXIS2_PLACEMENT_3D('',#6688,#5461,#5462);
#4623=AXIS2_PLACEMENT_3D('',#6689,#5463,#5464);
#4624=AXIS2_PLACEMENT_3D('',#6691,#5465,#5466);
#4625=AXIS2_PLACEMENT_3D('',#6694,#5468,#5469);
#4626=AXIS2_PLACEMENT_3D('',#6695,#5470,#5471);
#4627=AXIS2_PLACEMENT_3D('',#6697,#5472,#5473);
#4628=AXIS2_PLACEMENT_3D('',#6700,#5475,#5476);
#4629=AXIS2_PLACEMENT_3D('',#6701,#5477,#5478);
#4630=AXIS2_PLACEMENT_3D('',#6702,#5479,#5480);
#4631=AXIS2_PLACEMENT_3D('',#6703,#5481,#5482);
#4632=AXIS2_PLACEMENT_3D('',#6704,#5483,#5484);
#4633=AXIS2_PLACEMENT_3D('',#6706,#5485,#5486);
#4634=AXIS2_PLACEMENT_3D('',#6709,#5488,#5489);
#4635=AXIS2_PLACEMENT_3D('',#6710,#5490,#5491);
#4636=AXIS2_PLACEMENT_3D('',#6711,#5492,#5493);
#4637=AXIS2_PLACEMENT_3D('',#6712,#5494,#5495);
#4638=AXIS2_PLACEMENT_3D('',#6713,#5496,#5497);
#4639=AXIS2_PLACEMENT_3D('',#6715,#5498,#5499);
#4640=AXIS2_PLACEMENT_3D('',#6718,#5501,#5502);
#4641=AXIS2_PLACEMENT_3D('',#6719,#5503,#5504);
#4642=AXIS2_PLACEMENT_3D('',#6720,#5505,#5506);
#4643=AXIS2_PLACEMENT_3D('',#6721,#5507,#5508);
#4644=AXIS2_PLACEMENT_3D('',#6722,#5509,#5510);
#4645=AXIS2_PLACEMENT_3D('',#6731,#5515,#5516);
#4646=AXIS2_PLACEMENT_3D('',#6737,#5520,#5521);
#4647=AXIS2_PLACEMENT_3D('',#6743,#5525,#5526);
#4648=AXIS2_PLACEMENT_3D('',#6749,#5530,#5531);
#4649=AXIS2_PLACEMENT_3D('',#6755,#5535,#5536);
#4650=AXIS2_PLACEMENT_3D('',#6758,#5539,#5540);
#4651=AXIS2_PLACEMENT_3D('',#6759,#5541,#5542);
#4652=AXIS2_PLACEMENT_3D('',#6760,#5543,#5544);
#4653=AXIS2_PLACEMENT_3D('',#6762,#5545,#5546);
#4654=AXIS2_PLACEMENT_3D('',#6764,#5547,#5548);
#4655=AXIS2_PLACEMENT_3D('',#6765,#5549,#5550);
#4656=AXIS2_PLACEMENT_3D('',#6768,#5552,#5553);
#4657=AXIS2_PLACEMENT_3D('',#6769,#5554,#5555);
#4658=AXIS2_PLACEMENT_3D('',#6770,#5556,#5557);
#4659=AXIS2_PLACEMENT_3D('',#6772,#5558,#5559);
#4660=AXIS2_PLACEMENT_3D('',#6773,#5560,#5561);
#4661=AXIS2_PLACEMENT_3D('',#6775,#5562,#5563);
#4662=AXIS2_PLACEMENT_3D('',#6777,#5565,#5566);
#4663=AXIS2_PLACEMENT_3D('',#6779,#5567,#5568);
#4664=AXIS2_PLACEMENT_3D('',#6781,#5570,#5571);
#4665=AXIS2_PLACEMENT_3D('',#6783,#5572,#5573);
#4666=AXIS2_PLACEMENT_3D('',#6785,#5575,#5576);
#4667=AXIS2_PLACEMENT_3D('',#6787,#5577,#5578);
#4668=AXIS2_PLACEMENT_3D('',#6788,#5579,#5580);
#4669=AXIS2_PLACEMENT_3D('',#6790,#5581,#5582);
#4670=AXIS2_PLACEMENT_3D('',#6792,#5584,#5585);
#4671=AXIS2_PLACEMENT_3D('',#6794,#5587,#5588);
#4672=AXIS2_PLACEMENT_3D('',#6795,#5589,#5590);
#4673=AXIS2_PLACEMENT_3D('',#6797,#5591,#5592);
#4674=AXIS2_PLACEMENT_3D('',#6800,#5594,#5595);
#4675=AXIS2_PLACEMENT_3D('',#6801,#5596,#5597);
#4676=AXIS2_PLACEMENT_3D('',#6804,#5599,#5600);
#4677=AXIS2_PLACEMENT_3D('',#6805,#5601,#5602);
#4678=AXIS2_PLACEMENT_3D('',#6807,#5603,#5604);
#4679=AXIS2_PLACEMENT_3D('',#6808,#5605,#5606);
#4680=AXIS2_PLACEMENT_3D('',#6811,#5608,#5609);
#4681=AXIS2_PLACEMENT_3D('',#6812,#5610,#5611);
#4682=AXIS2_PLACEMENT_3D('',#6813,#5612,#5613);
#4683=AXIS2_PLACEMENT_3D('',#6814,#5614,#5615);
#4684=AXIS2_PLACEMENT_3D('',#6826,#5617,#5618);
#4685=AXIS2_PLACEMENT_3D('',#6842,#5619,#5620);
#4686=AXIS2_PLACEMENT_3D('',#6844,#5621,#5622);
#4687=AXIS2_PLACEMENT_3D('',#6870,#5624,#5625);
#4688=AXIS2_PLACEMENT_3D('',#6873,#5628,#5629);
#4689=AXIS2_PLACEMENT_3D('',#6875,#5631,#5632);
#4690=AXIS2_PLACEMENT_3D('',#6877,#5634,#5635);
#4691=AXIS2_PLACEMENT_3D('',#6879,#5636,#5637);
#4692=AXIS2_PLACEMENT_3D('',#6882,#5639,#5640);
#4693=AXIS2_PLACEMENT_3D('',#6883,#5641,#5642);
#4694=AXIS2_PLACEMENT_3D('',#6885,#5644,#5645);
#4695=AXIS2_PLACEMENT_3D('',#6887,#5647,#5648);
#4696=AXIS2_PLACEMENT_3D('',#6888,#5649,#5650);
#4697=AXIS2_PLACEMENT_3D('',#6889,#5651,#5652);
#4698=AXIS2_PLACEMENT_3D('',#6890,#5653,#5654);
#4699=AXIS2_PLACEMENT_3D('',#6891,#5655,#5656);
#4700=AXIS2_PLACEMENT_3D('',#6905,#5663,#5664);
#4701=AXIS2_PLACEMENT_3D('',#6906,#5665,#5666);
#4702=AXIS2_PLACEMENT_3D('',#6920,#5673,#5674);
#4703=AXIS2_PLACEMENT_3D('',#6921,#5675,#5676);
#4704=AXIS2_PLACEMENT_3D('',#6924,#5679,#5680);
#4705=AXIS2_PLACEMENT_3D('',#6926,#5682,#5683);
#4706=AXIS2_PLACEMENT_3D('',#6928,#5685,#5686);
#4707=AXIS2_PLACEMENT_3D('',#6930,#5688,#5689);
#4708=AXIS2_PLACEMENT_3D('',#6932,#5691,#5692);
#4709=AXIS2_PLACEMENT_3D('',#6933,#5693,#5694);
#4710=AXIS2_PLACEMENT_3D('',#6936,#5696,#5697);
#4711=AXIS2_PLACEMENT_3D('',#6937,#5698,#5699);
#4712=AXIS2_PLACEMENT_3D('',#6939,#5700,#5701);
#4713=AXIS2_PLACEMENT_3D('',#6941,#5702,#5703);
#4714=AXIS2_PLACEMENT_3D('',#6942,#5704,#5705);
#4715=AXIS2_PLACEMENT_3D('',#6944,#5707,#5708);
#4716=AXIS2_PLACEMENT_3D('',#6946,#5709,#5710);
#4717=AXIS2_PLACEMENT_3D('',#6948,#5712,#5713);
#4718=AXIS2_PLACEMENT_3D('',#6950,#5714,#5715);
#4719=AXIS2_PLACEMENT_3D('',#6952,#5717,#5718);
#4720=AXIS2_PLACEMENT_3D('',#6954,#5719,#5720);
#4721=AXIS2_PLACEMENT_3D('',#6955,#5721,#5722);
#4722=AXIS2_PLACEMENT_3D('',#6957,#5724,#5725);
#4723=AXIS2_PLACEMENT_3D('',#6958,#5726,#5727);
#4724=AXIS2_PLACEMENT_3D('',#6960,#5728,#5729);
#4725=AXIS2_PLACEMENT_3D('',#6961,#5730,#5731);
#4726=AXIS2_PLACEMENT_3D('',#6963,#5732,#5733);
#4727=AXIS2_PLACEMENT_3D('',#6965,#5735,#5736);
#4728=AXIS2_PLACEMENT_3D('',#6967,#5737,#5738);
#4729=AXIS2_PLACEMENT_3D('',#6969,#5740,#5741);
#4730=AXIS2_PLACEMENT_3D('',#6971,#5742,#5743);
#4731=AXIS2_PLACEMENT_3D('',#6973,#5745,#5746);
#4732=AXIS2_PLACEMENT_3D('',#6975,#5747,#5748);
#4733=AXIS2_PLACEMENT_3D('',#6976,#5749,#5750);
#4734=AXIS2_PLACEMENT_3D('',#6978,#5751,#5752);
#4735=AXIS2_PLACEMENT_3D('',#6980,#5754,#5755);
#4736=AXIS2_PLACEMENT_3D('',#6982,#5756,#5757);
#4737=AXIS2_PLACEMENT_3D('',#6984,#5759,#5760);
#4738=AXIS2_PLACEMENT_3D('',#6986,#5761,#5762);
#4739=AXIS2_PLACEMENT_3D('',#6988,#5764,#5765);
#4740=AXIS2_PLACEMENT_3D('',#6989,#5766,#5767);
#4741=AXIS2_PLACEMENT_3D('',#6998,#5772,#5773);
#4742=AXIS2_PLACEMENT_3D('',#7004,#5777,#5778);
#4743=AXIS2_PLACEMENT_3D('',#7010,#5782,#5783);
#4744=AXIS2_PLACEMENT_3D('',#7016,#5787,#5788);
#4745=AXIS2_PLACEMENT_3D('',#7022,#5792,#5793);
#4746=AXIS2_PLACEMENT_3D('',#7025,#5796,#5797);
#4747=AXIS2_PLACEMENT_3D('',#7026,#5798,#5799);
#4748=AXIS2_PLACEMENT_3D('',#7027,#5800,#5801);
#4749=AXIS2_PLACEMENT_3D('',#7028,#5802,#5803);
#4750=AXIS2_PLACEMENT_3D('',#7029,#5804,#5805);
#4751=AXIS2_PLACEMENT_3D('',#7030,#5806,#5807);
#4752=AXIS2_PLACEMENT_3D('',#7031,#5808,#5809);
#4753=AXIS2_PLACEMENT_3D('',#7032,#5810,#5811);
#4754=AXIS2_PLACEMENT_3D('',#7033,#5812,#5813);
#4755=AXIS2_PLACEMENT_3D('',#7034,#5814,#5815);
#4756=AXIS2_PLACEMENT_3D('',#7035,#5816,#5817);
#4757=AXIS2_PLACEMENT_3D('',#7036,#5818,#5819);
#4758=AXIS2_PLACEMENT_3D('',#7037,#5820,#5821);
#4759=AXIS2_PLACEMENT_3D('',#7038,#5822,#5823);
#4760=AXIS2_PLACEMENT_3D('',#7039,#5824,#5825);
#4761=AXIS2_PLACEMENT_3D('',#7040,#5826,#5827);
#4762=AXIS2_PLACEMENT_3D('',#7041,#5828,#5829);
#4763=AXIS2_PLACEMENT_3D('',#7042,#5830,#5831);
#4764=AXIS2_PLACEMENT_3D('',#7043,#5832,#5833);
#4765=AXIS2_PLACEMENT_3D('',#7044,#5834,#5835);
#4766=AXIS2_PLACEMENT_3D('',#7045,#5836,#5837);
#4767=AXIS2_PLACEMENT_3D('',#7046,#5838,#5839);
#4768=AXIS2_PLACEMENT_3D('',#7047,#5840,#5841);
#4769=AXIS2_PLACEMENT_3D('',#7048,#5842,#5843);
#4770=AXIS2_PLACEMENT_3D('',#7049,#5844,#5845);
#4771=AXIS2_PLACEMENT_3D('',#7050,#5846,#5847);
#4772=AXIS2_PLACEMENT_3D('',#7051,#5848,#5849);
#4773=AXIS2_PLACEMENT_3D('',#7052,#5850,#5851);
#4774=AXIS2_PLACEMENT_3D('',#7053,#5852,#5853);
#4775=AXIS2_PLACEMENT_3D('',#7054,#5854,#5855);
#4776=AXIS2_PLACEMENT_3D('',#7055,#5856,#5857);
#4777=AXIS2_PLACEMENT_3D('',#7056,#5858,#5859);
#4778=AXIS2_PLACEMENT_3D('',#7057,#5860,#5861);
#4779=AXIS2_PLACEMENT_3D('',#7058,#5862,#5863);
#4780=AXIS2_PLACEMENT_3D('',#7059,#5864,#5865);
#4781=AXIS2_PLACEMENT_3D('',#7060,#5866,#5867);
#4782=AXIS2_PLACEMENT_3D('',#7061,#5868,#5869);
#4783=AXIS2_PLACEMENT_3D('',#7062,#5870,#5871);
#4784=AXIS2_PLACEMENT_3D('',#7063,#5872,#5873);
#4785=AXIS2_PLACEMENT_3D('',#7064,#5874,#5875);
#4786=AXIS2_PLACEMENT_3D('',#7065,#5876,#5877);
#4787=AXIS2_PLACEMENT_3D('',#7066,#5878,#5879);
#4788=AXIS2_PLACEMENT_3D('',#7069,#5880,#5881);
#4789=AXIS2_PLACEMENT_3D('',#7075,#5885,#5886);
#4790=AXIS2_PLACEMENT_3D('',#7077,#5887,#5888);
#4791=AXIS2_PLACEMENT_3D('',#7082,#5891,#5892);
#4792=AXIS2_PLACEMENT_3D('',#7083,#5893,#5894);
#4793=AXIS2_PLACEMENT_3D('',#7085,#5895,#5896);
#4794=AXIS2_PLACEMENT_3D('',#7089,#5899,#5900);
#4795=AXIS2_PLACEMENT_3D('',#7090,#5901,#5902);
#4796=AXIS2_PLACEMENT_3D('',#7092,#5904,#5905);
#4797=AXIS2_PLACEMENT_3D('',#7093,#5906,#5907);
#4798=AXIS2_PLACEMENT_3D('',#7095,#5908,#5909);
#4799=AXIS2_PLACEMENT_3D('',#7098,#5911,#5912);
#4800=AXIS2_PLACEMENT_3D('',#7099,#5913,#5914);
#4801=AXIS2_PLACEMENT_3D('',#7101,#5915,#5916);
#4802=AXIS2_PLACEMENT_3D('',#7102,#5917,#5918);
#4803=AXIS2_PLACEMENT_3D('',#7103,#5919,#5920);
#4804=AXIS2_PLACEMENT_3D('',#7105,#5921,#5922);
#4805=AXIS2_PLACEMENT_3D('',#7108,#5924,#5925);
#4806=AXIS2_PLACEMENT_3D('',#7109,#5926,#5927);
#4807=AXIS2_PLACEMENT_3D('',#7110,#5928,#5929);
#4808=AXIS2_PLACEMENT_3D('',#7113,#5930,#5931);
#4809=AXIS2_PLACEMENT_3D('',#7117,#5934,#5935);
#4810=AXIS2_PLACEMENT_3D('',#7120,#5936,#5937);
#4811=AXIS2_PLACEMENT_3D('',#7124,#5940,#5941);
#4812=AXIS2_PLACEMENT_3D('',#7127,#5942,#5943);
#4813=AXIS2_PLACEMENT_3D('',#7131,#5946,#5947);
#4814=AXIS2_PLACEMENT_3D('',#7134,#5948,#5949);
#4815=AXIS2_PLACEMENT_3D('',#7138,#5952,#5953);
#4816=AXIS2_PLACEMENT_3D('',#7145,#5958,#5959);
#4817=AXIS2_PLACEMENT_3D('',#7150,#5963,#5964);
#4818=AXIS2_PLACEMENT_3D('',#7155,#5968,#5969);
#4819=AXIS2_PLACEMENT_3D('',#7158,#5972,#5973);
#4820=AXIS2_PLACEMENT_3D('',#7159,#5974,#5975);
#4821=AXIS2_PLACEMENT_3D('',#7160,#5976,#5977);
#4822=AXIS2_PLACEMENT_3D('',#7161,#5978,#5979);
#4823=AXIS2_PLACEMENT_3D('',#7163,#5980,#5981);
#4824=AXIS2_PLACEMENT_3D('',#7164,#5982,#5983);
#4825=AXIS2_PLACEMENT_3D('',#7165,#5984,#5985);
#4826=AXIS2_PLACEMENT_3D('',#7166,#5986,#5987);
#4827=AXIS2_PLACEMENT_3D('',#7167,#5988,#5989);
#4828=AXIS2_PLACEMENT_3D('',#7168,#5990,#5991);
#4829=AXIS2_PLACEMENT_3D('',#7169,#5992,#5993);
#4830=AXIS2_PLACEMENT_3D('',#7178,#5998,#5999);
#4831=AXIS2_PLACEMENT_3D('',#7184,#6003,#6004);
#4832=AXIS2_PLACEMENT_3D('',#7190,#6008,#6009);
#4833=AXIS2_PLACEMENT_3D('',#7193,#6012,#6013);
#4834=AXIS2_PLACEMENT_3D('',#7194,#6014,#6015);
#4835=AXIS2_PLACEMENT_3D('',#7197,#6017,#6018);
#4836=AXIS2_PLACEMENT_3D('',#7198,#6019,#6020);
#4837=AXIS2_PLACEMENT_3D('',#7199,#6021,#6022);
#4838=AXIS2_PLACEMENT_3D('',#7200,#6023,#6024);
#4839=AXIS2_PLACEMENT_3D('',#7209,#6029,#6030);
#4840=AXIS2_PLACEMENT_3D('',#7215,#6034,#6035);
#4841=AXIS2_PLACEMENT_3D('',#7221,#6039,#6040);
#4842=AXIS2_PLACEMENT_3D('',#7224,#6043,#6044);
#4843=AXIS2_PLACEMENT_3D('',#7233,#6049,#6050);
#4844=AXIS2_PLACEMENT_3D('',#7239,#6054,#6055);
#4845=AXIS2_PLACEMENT_3D('',#7245,#6059,#6060);
#4846=AXIS2_PLACEMENT_3D('',#7248,#6063,#6064);
#4847=AXIS2_PLACEMENT_3D('',#7249,#6065,#6066);
#4848=AXIS2_PLACEMENT_3D('',#7250,#6067,#6068);
#4849=AXIS2_PLACEMENT_3D('',#7251,#6069,#6070);
#4850=AXIS2_PLACEMENT_3D('',#7253,#6071,#6072);
#4851=AXIS2_PLACEMENT_3D('',#7256,#6074,#6075);
#4852=AXIS2_PLACEMENT_3D('',#7257,#6076,#6077);
#4853=AXIS2_PLACEMENT_3D('',#7259,#6078,#6079);
#4854=AXIS2_PLACEMENT_3D('',#7262,#6081,#6082);
#4855=AXIS2_PLACEMENT_3D('',#7263,#6083,#6084);
#4856=AXIS2_PLACEMENT_3D('',#7264,#6085,#6086);
#4857=AXIS2_PLACEMENT_3D('',#7265,#6087,#6088);
#4858=AXIS2_PLACEMENT_3D('',#7266,#6089,#6090);
#4859=AXIS2_PLACEMENT_3D('',#7275,#6095,#6096);
#4860=AXIS2_PLACEMENT_3D('',#7281,#6100,#6101);
#4861=AXIS2_PLACEMENT_3D('',#7287,#6105,#6106);
#4862=AXIS2_PLACEMENT_3D('',#7290,#6109,#6110);
#4863=AXIS2_PLACEMENT_3D('',#7291,#6111,#6112);
#4864=AXIS2_PLACEMENT_3D('',#7292,#6113,#6114);
#4865=AXIS2_PLACEMENT_3D('',#7293,#6115,#6116);
#4866=AXIS2_PLACEMENT_3D('',#7302,#6121,#6122);
#4867=AXIS2_PLACEMENT_3D('',#7308,#6126,#6127);
#4868=AXIS2_PLACEMENT_3D('',#7314,#6131,#6132);
#4869=AXIS2_PLACEMENT_3D('',#7320,#6136,#6137);
#4870=AXIS2_PLACEMENT_3D('',#7326,#6141,#6142);
#4871=AXIS2_PLACEMENT_3D('',#7329,#6145,#6146);
#4872=AXIS2_PLACEMENT_3D('',#7330,#6147,#6148);
#4873=AXIS2_PLACEMENT_3D('',#7331,#6149,#6150);
#4874=AXIS2_PLACEMENT_3D('',#7333,#6151,#6152);
#4875=AXIS2_PLACEMENT_3D('',#7334,#6153,#6154);
#4876=AXIS2_PLACEMENT_3D('',#7336,#6155,#6156);
#4877=AXIS2_PLACEMENT_3D('',#7337,#6157,#6158);
#4878=AXIS2_PLACEMENT_3D('',#7339,#6159,#6160);
#4879=AXIS2_PLACEMENT_3D('',#7341,#6162,#6163);
#4880=AXIS2_PLACEMENT_3D('',#7343,#6164,#6165);
#4881=AXIS2_PLACEMENT_3D('',#7345,#6167,#6168);
#4882=AXIS2_PLACEMENT_3D('',#7347,#6169,#6170);
#4883=AXIS2_PLACEMENT_3D('',#7349,#6172,#6173);
#4884=AXIS2_PLACEMENT_3D('',#7351,#6174,#6175);
#4885=AXIS2_PLACEMENT_3D('',#7352,#6176,#6177);
#4886=AXIS2_PLACEMENT_3D('',#7354,#6178,#6179);
#4887=AXIS2_PLACEMENT_3D('',#7356,#6181,#6182);
#4888=AXIS2_PLACEMENT_3D('',#7358,#6184,#6185);
#4889=AXIS2_PLACEMENT_3D('',#7359,#6186,#6187);
#4890=AXIS2_PLACEMENT_3D('',#7360,#6188,#6189);
#4891=AXIS2_PLACEMENT_3D('',#7361,#6190,#6191);
#4892=AXIS2_PLACEMENT_3D('',#7362,#6192,#6193);
#4893=AXIS2_PLACEMENT_3D('',#7363,#6194,#6195);
#4894=AXIS2_PLACEMENT_3D('',#7364,#6196,#6197);
#4895=AXIS2_PLACEMENT_3D('',#7365,#6198,#6199);
#4896=DIRECTION('axis',(0.,0.,1.));
#4897=DIRECTION('refdir',(1.,0.,0.));
#4898=DIRECTION('axis',(0.,0.,1.));
#4899=DIRECTION('refdir',(1.,0.,0.));
#4900=DIRECTION('axis',(0.,0.,1.));
#4901=DIRECTION('refdir',(1.,0.,0.));
#4902=DIRECTION('center_axis',(0.,0.,1.));
#4903=DIRECTION('ref_axis',(1.,0.,0.));
#4904=DIRECTION('center_axis',(0.,0.,1.));
#4905=DIRECTION('ref_axis',(1.,0.,0.));
#4906=DIRECTION('',(0.,0.,1.));
#4907=DIRECTION('center_axis',(0.,0.,-1.));
#4908=DIRECTION('ref_axis',(1.,0.,0.));
#4909=DIRECTION('center_axis',(0.,0.,1.));
#4910=DIRECTION('ref_axis',(1.,0.,0.));
#4911=DIRECTION('center_axis',(0.,0.,1.));
#4912=DIRECTION('ref_axis',(1.,0.,0.));
#4913=DIRECTION('center_axis',(0.,0.,1.));
#4914=DIRECTION('ref_axis',(1.,0.,0.));
#4915=DIRECTION('',(0.,0.,1.));
#4916=DIRECTION('center_axis',(0.,0.,-1.));
#4917=DIRECTION('ref_axis',(1.,0.,0.));
#4918=DIRECTION('center_axis',(0.,0.,1.));
#4919=DIRECTION('ref_axis',(1.,0.,0.));
#4920=DIRECTION('center_axis',(0.,1.,0.));
#4921=DIRECTION('ref_axis',(1.,0.,0.));
#4922=DIRECTION('center_axis',(0.,1.,0.));
#4923=DIRECTION('ref_axis',(1.,0.,0.));
#4924=DIRECTION('',(0.,1.,0.));
#4925=DIRECTION('center_axis',(0.,-1.,0.));
#4926=DIRECTION('ref_axis',(1.,0.,0.));
#4927=DIRECTION('center_axis',(0.,1.,0.));
#4928=DIRECTION('ref_axis',(1.,0.,0.));
#4929=DIRECTION('center_axis',(0.,1.,0.));
#4930=DIRECTION('ref_axis',(1.,0.,0.));
#4931=DIRECTION('',(0.,1.,0.));
#4932=DIRECTION('center_axis',(0.,-1.,0.));
#4933=DIRECTION('ref_axis',(1.,0.,0.));
#4934=DIRECTION('center_axis',(0.,1.,0.));
#4935=DIRECTION('ref_axis',(1.,0.,0.));
#4936=DIRECTION('center_axis',(0.,1.,0.));
#4937=DIRECTION('ref_axis',(1.,0.,0.));
#4938=DIRECTION('',(0.,1.,0.));
#4939=DIRECTION('center_axis',(0.,-1.,0.));
#4940=DIRECTION('ref_axis',(1.,0.,0.));
#4941=DIRECTION('center_axis',(0.,1.,0.));
#4942=DIRECTION('ref_axis',(1.,0.,0.));
#4943=DIRECTION('center_axis',(0.,1.,0.));
#4944=DIRECTION('ref_axis',(1.,0.,0.));
#4945=DIRECTION('',(0.,1.,0.));
#4946=DIRECTION('center_axis',(0.,-1.,0.));
#4947=DIRECTION('ref_axis',(1.,0.,0.));
#4948=DIRECTION('center_axis',(0.,0.,1.));
#4949=DIRECTION('ref_axis',(1.,0.,0.));
#4950=DIRECTION('',(0.,0.,1.));
#4951=DIRECTION('center_axis',(0.,0.,1.));
#4952=DIRECTION('ref_axis',(1.,0.,0.));
#4953=DIRECTION('',(0.,0.,-1.));
#4954=DIRECTION('center_axis',(0.,0.,-1.));
#4955=DIRECTION('ref_axis',(1.,0.,0.));
#4956=DIRECTION('center_axis',(0.,0.,1.));
#4957=DIRECTION('ref_axis',(1.,0.,0.));
#4958=DIRECTION('',(1.,0.,0.));
#4959=DIRECTION('center_axis',(0.,0.,1.));
#4960=DIRECTION('ref_axis',(0.,-1.,0.));
#4961=DIRECTION('',(1.,0.,0.));
#4962=DIRECTION('center_axis',(0.,0.,1.));
#4963=DIRECTION('ref_axis',(1.,0.,0.));
#4964=DIRECTION('',(-1.,0.,0.));
#4965=DIRECTION('',(0.,-1.,0.));
#4966=DIRECTION('',(1.,0.,0.));
#4967=DIRECTION('',(0.,1.,0.));
#4968=DIRECTION('',(-1.,0.,0.));
#4969=DIRECTION('center_axis',(0.,1.,0.));
#4970=DIRECTION('ref_axis',(1.,0.,0.));
#4971=DIRECTION('center_axis',(0.,1.,0.));
#4972=DIRECTION('ref_axis',(1.,0.,0.));
#4973=DIRECTION('',(0.,1.,0.));
#4974=DIRECTION('center_axis',(0.,-1.,0.));
#4975=DIRECTION('ref_axis',(1.,0.,0.));
#4976=DIRECTION('center_axis',(0.,1.,0.));
#4977=DIRECTION('ref_axis',(1.,0.,0.));
#4978=DIRECTION('center_axis',(0.,1.,0.));
#4979=DIRECTION('ref_axis',(1.,0.,0.));
#4980=DIRECTION('',(0.,1.,0.));
#4981=DIRECTION('center_axis',(0.,1.,0.));
#4982=DIRECTION('ref_axis',(1.,0.,0.));
#4983=DIRECTION('center_axis',(0.,1.,0.));
#4984=DIRECTION('ref_axis',(1.,0.,0.));
#4985=DIRECTION('center_axis',(0.,-1.,0.));
#4986=DIRECTION('ref_axis',(0.,0.,-1.));
#4987=DIRECTION('center_axis',(0.,1.,0.));
#4988=DIRECTION('ref_axis',(1.,0.,0.));
#4989=DIRECTION('center_axis',(6.12323399573677E-17,0.,1.));
#4990=DIRECTION('ref_axis',(1.,0.,0.));
#4991=DIRECTION('center_axis',(0.,-1.,0.));
#4992=DIRECTION('ref_axis',(0.,0.,-1.));
#4993=DIRECTION('center_axis',(0.,1.,0.));
#4994=DIRECTION('ref_axis',(-1.,0.,0.));
#4995=DIRECTION('',(0.,0.,1.));
#4996=DIRECTION('',(-1.,0.,0.));
#4997=DIRECTION('',(0.,0.,1.));
#4998=DIRECTION('center_axis',(1.,0.,0.));
#4999=DIRECTION('ref_axis',(0.,1.,0.));
#5000=DIRECTION('',(0.,1.,0.));
#5001=DIRECTION('',(0.,0.,1.));
#5002=DIRECTION('center_axis',(0.,-1.,0.));
#5003=DIRECTION('ref_axis',(1.,0.,0.));
#5004=DIRECTION('',(1.,0.,0.));
#5005=DIRECTION('',(0.,0.,1.));
#5006=DIRECTION('center_axis',(-1.,0.,0.));
#5007=DIRECTION('ref_axis',(0.,-1.,0.));
#5008=DIRECTION('',(0.,-1.,0.));
#5009=DIRECTION('center_axis',(0.,0.,1.));
#5010=DIRECTION('ref_axis',(1.,0.,0.));
#5011=DIRECTION('axis',(0.,0.,1.));
#5012=DIRECTION('refdir',(1.,0.,0.));
#5013=DIRECTION('center_axis',(6.12323399573677E-17,0.,1.));
#5014=DIRECTION('ref_axis',(1.,0.,0.));
#5015=DIRECTION('center_axis',(0.,-1.,0.));
#5016=DIRECTION('ref_axis',(0.,0.,-1.));
#5017=DIRECTION('center_axis',(0.,1.,0.));
#5018=DIRECTION('ref_axis',(1.,0.,0.));
#5019=DIRECTION('center_axis',(0.,1.,0.));
#5020=DIRECTION('ref_axis',(1.,0.,0.));
#5021=DIRECTION('',(0.,-1.,0.));
#5022=DIRECTION('center_axis',(0.,-1.,0.));
#5023=DIRECTION('ref_axis',(1.,0.,0.));
#5024=DIRECTION('center_axis',(0.,1.,0.));
#5025=DIRECTION('ref_axis',(1.,0.,0.));
#5026=DIRECTION('center_axis',(0.,1.,0.));
#5027=DIRECTION('ref_axis',(1.,0.,0.));
#5028=DIRECTION('',(0.,-1.,0.));
#5029=DIRECTION('center_axis',(0.,1.,0.));
#5030=DIRECTION('ref_axis',(1.,0.,0.));
#5031=DIRECTION('center_axis',(0.,1.,0.));
#5032=DIRECTION('ref_axis',(1.,0.,0.));
#5033=DIRECTION('center_axis',(0.,1.,0.));
#5034=DIRECTION('ref_axis',(1.,0.,0.));
#5035=DIRECTION('axis',(0.,0.,1.));
#5036=DIRECTION('refdir',(1.,0.,0.));
#5037=DIRECTION('center_axis',(0.,0.,1.));
#5038=DIRECTION('ref_axis',(1.,0.,0.));
#5039=DIRECTION('center_axis',(0.,0.,1.));
#5040=DIRECTION('ref_axis',(1.,0.,0.));
#5041=DIRECTION('',(0.,0.,1.));
#5042=DIRECTION('center_axis',(0.,0.,-1.));
#5043=DIRECTION('ref_axis',(1.,0.,0.));
#5044=DIRECTION('center_axis',(0.,0.,1.));
#5045=DIRECTION('ref_axis',(1.,0.,0.));
#5046=DIRECTION('center_axis',(0.,0.,1.));
#5047=DIRECTION('ref_axis',(1.,0.,0.));
#5048=DIRECTION('center_axis',(0.,0.,1.));
#5049=DIRECTION('ref_axis',(1.,0.,0.));
#5050=DIRECTION('',(0.,0.,1.));
#5051=DIRECTION('center_axis',(0.,0.,-1.));
#5052=DIRECTION('ref_axis',(1.,0.,0.));
#5053=DIRECTION('center_axis',(0.,0.,1.));
#5054=DIRECTION('ref_axis',(1.,0.,0.));
#5055=DIRECTION('center_axis',(0.,1.,0.));
#5056=DIRECTION('ref_axis',(1.,0.,0.));
#5057=DIRECTION('center_axis',(0.,1.,0.));
#5058=DIRECTION('ref_axis',(1.,0.,0.));
#5059=DIRECTION('',(0.,1.,0.));
#5060=DIRECTION('center_axis',(0.,-1.,0.));
#5061=DIRECTION('ref_axis',(1.,0.,0.));
#5062=DIRECTION('center_axis',(0.,1.,0.));
#5063=DIRECTION('ref_axis',(1.,0.,0.));
#5064=DIRECTION('center_axis',(0.,1.,0.));
#5065=DIRECTION('ref_axis',(1.,0.,0.));
#5066=DIRECTION('',(0.,1.,0.));
#5067=DIRECTION('center_axis',(0.,-1.,0.));
#5068=DIRECTION('ref_axis',(1.,0.,0.));
#5069=DIRECTION('center_axis',(0.,1.,0.));
#5070=DIRECTION('ref_axis',(1.,0.,0.));
#5071=DIRECTION('center_axis',(0.,1.,0.));
#5072=DIRECTION('ref_axis',(1.,0.,0.));
#5073=DIRECTION('',(0.,1.,0.));
#5074=DIRECTION('center_axis',(0.,-1.,0.));
#5075=DIRECTION('ref_axis',(1.,0.,0.));
#5076=DIRECTION('center_axis',(0.,1.,0.));
#5077=DIRECTION('ref_axis',(1.,0.,0.));
#5078=DIRECTION('center_axis',(0.,1.,0.));
#5079=DIRECTION('ref_axis',(1.,0.,0.));
#5080=DIRECTION('',(0.,1.,0.));
#5081=DIRECTION('center_axis',(0.,-1.,0.));
#5082=DIRECTION('ref_axis',(1.,0.,0.));
#5083=DIRECTION('center_axis',(0.,0.,1.));
#5084=DIRECTION('ref_axis',(1.,0.,0.));
#5085=DIRECTION('',(0.,0.,1.));
#5086=DIRECTION('center_axis',(0.,0.,1.));
#5087=DIRECTION('ref_axis',(1.,0.,0.));
#5088=DIRECTION('',(0.,0.,-1.));
#5089=DIRECTION('center_axis',(0.,0.,-1.));
#5090=DIRECTION('ref_axis',(1.,0.,0.));
#5091=DIRECTION('center_axis',(0.,0.,1.));
#5092=DIRECTION('ref_axis',(1.,0.,0.));
#5093=DIRECTION('',(-1.,0.,0.));
#5094=DIRECTION('center_axis',(0.,0.,1.));
#5095=DIRECTION('ref_axis',(0.,-1.,0.));
#5096=DIRECTION('',(-1.,0.,0.));
#5097=DIRECTION('center_axis',(0.,0.,1.));
#5098=DIRECTION('ref_axis',(1.,0.,0.));
#5099=DIRECTION('',(1.,0.,0.));
#5100=DIRECTION('',(0.,1.,0.));
#5101=DIRECTION('',(-1.,0.,0.));
#5102=DIRECTION('',(0.,-1.,0.));
#5103=DIRECTION('',(1.,0.,0.));
#5104=DIRECTION('center_axis',(0.,1.,0.));
#5105=DIRECTION('ref_axis',(1.,0.,0.));
#5106=DIRECTION('center_axis',(0.,1.,0.));
#5107=DIRECTION('ref_axis',(1.,0.,0.));
#5108=DIRECTION('',(0.,1.,0.));
#5109=DIRECTION('center_axis',(0.,-1.,0.));
#5110=DIRECTION('ref_axis',(1.,0.,0.));
#5111=DIRECTION('center_axis',(0.,1.,0.));
#5112=DIRECTION('ref_axis',(1.,0.,0.));
#5113=DIRECTION('center_axis',(0.,1.,0.));
#5114=DIRECTION('ref_axis',(1.,0.,0.));
#5115=DIRECTION('',(0.,1.,0.));
#5116=DIRECTION('center_axis',(0.,1.,0.));
#5117=DIRECTION('ref_axis',(1.,0.,0.));
#5118=DIRECTION('center_axis',(0.,1.,0.));
#5119=DIRECTION('ref_axis',(1.,0.,0.));
#5120=DIRECTION('center_axis',(0.,1.,0.));
#5121=DIRECTION('ref_axis',(1.,0.,0.));
#5122=DIRECTION('center_axis',(0.,1.,0.));
#5123=DIRECTION('ref_axis',(0.,0.,1.));
#5124=DIRECTION('center_axis',(6.12323399573677E-17,0.,1.));
#5125=DIRECTION('ref_axis',(1.,0.,0.));
#5126=DIRECTION('center_axis',(0.,1.,0.));
#5127=DIRECTION('ref_axis',(0.,0.,1.));
#5128=DIRECTION('center_axis',(0.,1.,0.));
#5129=DIRECTION('ref_axis',(-1.,0.,0.));
#5130=DIRECTION('',(-1.,0.,0.));
#5131=DIRECTION('',(0.,0.,1.));
#5132=DIRECTION('',(0.,0.,1.));
#5133=DIRECTION('center_axis',(1.,0.,0.));
#5134=DIRECTION('ref_axis',(0.,1.,0.));
#5135=DIRECTION('',(0.,1.,0.));
#5136=DIRECTION('',(0.,0.,1.));
#5137=DIRECTION('center_axis',(0.,-1.,0.));
#5138=DIRECTION('ref_axis',(1.,0.,0.));
#5139=DIRECTION('',(0.,0.,1.));
#5140=DIRECTION('',(1.,0.,0.));
#5141=DIRECTION('center_axis',(-1.,0.,0.));
#5142=DIRECTION('ref_axis',(0.,-1.,0.));
#5143=DIRECTION('',(0.,-1.,0.));
#5144=DIRECTION('center_axis',(0.,0.,1.));
#5145=DIRECTION('ref_axis',(1.,0.,0.));
#5146=DIRECTION('axis',(0.,0.,1.));
#5147=DIRECTION('refdir',(1.,0.,0.));
#5148=DIRECTION('center_axis',(6.12323399573677E-17,0.,1.));
#5149=DIRECTION('ref_axis',(1.,0.,0.));
#5150=DIRECTION('center_axis',(0.,1.,0.));
#5151=DIRECTION('ref_axis',(0.,0.,1.));
#5152=DIRECTION('center_axis',(0.,-1.,0.));
#5153=DIRECTION('ref_axis',(1.,0.,0.));
#5154=DIRECTION('center_axis',(0.,1.,0.));
#5155=DIRECTION('ref_axis',(1.,0.,0.));
#5156=DIRECTION('center_axis',(0.,-1.,0.));
#5157=DIRECTION('ref_axis',(1.,0.,0.));
#5158=DIRECTION('',(0.,-1.,0.));
#5159=DIRECTION('center_axis',(0.,1.,0.));
#5160=DIRECTION('ref_axis',(1.,0.,0.));
#5161=DIRECTION('center_axis',(0.,1.,0.));
#5162=DIRECTION('ref_axis',(1.,0.,0.));
#5163=DIRECTION('',(0.,-1.,0.));
#5164=DIRECTION('center_axis',(0.,1.,0.));
#5165=DIRECTION('ref_axis',(1.,0.,0.));
#5166=DIRECTION('center_axis',(0.,1.,0.));
#5167=DIRECTION('ref_axis',(1.,0.,0.));
#5168=DIRECTION('center_axis',(0.,1.,0.));
#5169=DIRECTION('ref_axis',(1.,0.,0.));
#5170=DIRECTION('axis',(0.,0.,1.));
#5171=DIRECTION('refdir',(1.,0.,0.));
#5172=DIRECTION('center_axis',(0.,1.,0.));
#5173=DIRECTION('ref_axis',(1.,0.,0.));
#5174=DIRECTION('center_axis',(0.,1.,0.));
#5175=DIRECTION('ref_axis',(1.,0.,0.));
#5176=DIRECTION('',(0.,1.,0.));
#5177=DIRECTION('center_axis',(0.,-1.,0.));
#5178=DIRECTION('ref_axis',(1.,0.,0.));
#5179=DIRECTION('center_axis',(0.,1.,0.));
#5180=DIRECTION('ref_axis',(1.,0.,0.));
#5181=DIRECTION('center_axis',(0.,1.,0.));
#5182=DIRECTION('ref_axis',(1.,0.,0.));
#5183=DIRECTION('',(0.,1.,0.));
#5184=DIRECTION('center_axis',(0.,-1.,0.));
#5185=DIRECTION('ref_axis',(1.,0.,0.));
#5186=DIRECTION('center_axis',(0.,1.,0.));
#5187=DIRECTION('ref_axis',(1.,0.,0.));
#5188=DIRECTION('center_axis',(0.,1.,0.));
#5189=DIRECTION('ref_axis',(1.,0.,0.));
#5190=DIRECTION('',(0.,1.,0.));
#5191=DIRECTION('center_axis',(0.,-1.,0.));
#5192=DIRECTION('ref_axis',(1.,0.,0.));
#5193=DIRECTION('center_axis',(0.,1.,0.));
#5194=DIRECTION('ref_axis',(1.,0.,0.));
#5195=DIRECTION('center_axis',(0.,1.,0.));
#5196=DIRECTION('ref_axis',(1.,0.,0.));
#5197=DIRECTION('',(0.,1.,0.));
#5198=DIRECTION('center_axis',(0.,-1.,0.));
#5199=DIRECTION('ref_axis',(1.,0.,0.));
#5200=DIRECTION('center_axis',(-1.,0.,0.));
#5201=DIRECTION('ref_axis',(0.,0.,1.));
#5202=DIRECTION('',(0.,0.,1.));
#5203=DIRECTION('',(0.,1.,0.));
#5204=DIRECTION('',(0.,0.,-1.));
#5205=DIRECTION('',(0.,1.,0.));
#5206=DIRECTION('center_axis',(0.,0.,-1.));
#5207=DIRECTION('ref_axis',(-1.,0.,0.));
#5208=DIRECTION('',(-1.,0.,0.));
#5209=DIRECTION('',(0.,1.,0.));
#5210=DIRECTION('',(1.,0.,0.));
#5211=DIRECTION('',(0.,1.,0.));
#5212=DIRECTION('center_axis',(0.,0.,-1.));
#5213=DIRECTION('ref_axis',(-1.,0.,0.));
#5214=DIRECTION('',(-1.,0.,0.));
#5215=DIRECTION('',(0.,-1.,0.));
#5216=DIRECTION('',(1.,0.,0.));
#5217=DIRECTION('center_axis',(1.,0.,0.));
#5218=DIRECTION('ref_axis',(0.,0.,-1.));
#5219=DIRECTION('',(0.,0.,-1.));
#5220=DIRECTION('',(0.,-1.,0.));
#5221=DIRECTION('',(0.,0.,1.));
#5222=DIRECTION('center_axis',(0.,1.,0.));
#5223=DIRECTION('ref_axis',(0.,0.,1.));
#5224=DIRECTION('center_axis',(0.,-1.,0.));
#5225=DIRECTION('ref_axis',(1.,0.,0.));
#5226=DIRECTION('',(1.,0.,0.));
#5227=DIRECTION('',(0.,0.,-1.));
#5228=DIRECTION('',(-1.,0.,0.));
#5229=DIRECTION('',(0.,0.,1.));
#5230=DIRECTION('',(1.,0.,0.));
#5231=DIRECTION('center_axis',(0.,0.,1.));
#5232=DIRECTION('ref_axis',(1.,0.,0.));
#5233=DIRECTION('',(-1.,0.,0.));
#5234=DIRECTION('',(0.,1.,0.));
#5235=DIRECTION('center_axis',(0.,0.,1.));
#5236=DIRECTION('ref_axis',(1.,0.,0.));
#5237=DIRECTION('',(0.,1.,0.));
#5238=DIRECTION('',(-1.,0.,0.));
#5239=DIRECTION('center_axis',(0.,1.,0.));
#5240=DIRECTION('ref_axis',(-1.83697019872103E-16,0.,-1.));
#5241=DIRECTION('center_axis',(0.,1.,0.));
#5242=DIRECTION('ref_axis',(1.,0.,0.));
#5243=DIRECTION('center_axis',(-1.,0.,0.));
#5244=DIRECTION('ref_axis',(0.,0.,1.));
#5245=DIRECTION('',(0.,0.,-1.));
#5246=DIRECTION('',(0.,1.,0.));
#5247=DIRECTION('center_axis',(0.,0.,-1.));
#5248=DIRECTION('ref_axis',(-1.,0.,0.));
#5249=DIRECTION('',(1.,0.,0.));
#5250=DIRECTION('',(0.,1.,0.));
#5251=DIRECTION('center_axis',(1.,0.,0.));
#5252=DIRECTION('ref_axis',(0.,0.,-1.));
#5253=DIRECTION('',(0.,0.,1.));
#5254=DIRECTION('center_axis',(0.,1.,0.));
#5255=DIRECTION('ref_axis',(1.,0.,0.));
#5256=DIRECTION('axis',(0.,0.,1.));
#5257=DIRECTION('refdir',(1.,0.,0.));
#5258=DIRECTION('center_axis',(0.,0.,1.));
#5259=DIRECTION('ref_axis',(1.,0.,0.));
#5260=DIRECTION('center_axis',(0.,0.,1.));
#5261=DIRECTION('ref_axis',(1.,0.,0.));
#5262=DIRECTION('center_axis',(0.,0.,1.));
#5263=DIRECTION('ref_axis',(1.,0.,0.));
#5264=DIRECTION('center_axis',(0.,0.,1.));
#5265=DIRECTION('ref_axis',(1.,0.,0.));
#5266=DIRECTION('center_axis',(0.,0.,1.));
#5267=DIRECTION('ref_axis',(1.,0.,0.));
#5268=DIRECTION('',(0.,0.,-1.));
#5269=DIRECTION('center_axis',(0.,0.,1.));
#5270=DIRECTION('ref_axis',(1.,0.,0.));
#5271=DIRECTION('center_axis',(0.,0.,-1.));
#5272=DIRECTION('ref_axis',(1.,0.,0.));
#5273=DIRECTION('center_axis',(0.,0.,1.));
#5274=DIRECTION('ref_axis',(1.,0.,0.));
#5275=DIRECTION('',(0.,0.,-1.));
#5276=DIRECTION('center_axis',(0.,0.,-1.));
#5277=DIRECTION('ref_axis',(1.,0.,0.));
#5278=DIRECTION('center_axis',(0.,0.,1.));
#5279=DIRECTION('ref_axis',(1.,0.,0.));
#5280=DIRECTION('',(0.,0.,-1.));
#5281=DIRECTION('center_axis',(0.,0.,1.));
#5282=DIRECTION('ref_axis',(1.,0.,0.));
#5283=DIRECTION('center_axis',(0.,0.,1.));
#5284=DIRECTION('ref_axis',(1.,0.,0.));
#5285=DIRECTION('axis',(0.,0.,1.));
#5286=DIRECTION('refdir',(1.,0.,0.));
#5287=DIRECTION('center_axis',(0.,0.,1.));
#5288=DIRECTION('ref_axis',(1.,0.,0.));
#5289=DIRECTION('center_axis',(1.22464679914735E-16,-1.,0.));
#5290=DIRECTION('ref_axis',(-1.,-1.22464679914735E-16,0.));
#5291=DIRECTION('center_axis',(0.,0.,-1.));
#5292=DIRECTION('ref_axis',(1.,0.,0.));
#5293=DIRECTION('axis',(0.,0.,1.));
#5294=DIRECTION('refdir',(1.,0.,0.));
#5295=DIRECTION('center_axis',(0.,0.,1.));
#5296=DIRECTION('ref_axis',(1.,0.,0.));
#5297=DIRECTION('center_axis',(0.,0.,1.));
#5298=DIRECTION('ref_axis',(1.,0.,0.));
#5299=DIRECTION('',(0.,0.,1.));
#5300=DIRECTION('center_axis',(0.,0.,1.));
#5301=DIRECTION('ref_axis',(1.,0.,0.));
#5302=DIRECTION('center_axis',(0.,0.,1.));
#5303=DIRECTION('ref_axis',(1.,0.,0.));
#5304=DIRECTION('center_axis',(0.,0.,-1.));
#5305=DIRECTION('ref_axis',(1.,0.,0.));
#5306=DIRECTION('center_axis',(0.,0.,1.));
#5307=DIRECTION('ref_axis',(1.,0.,0.));
#5308=DIRECTION('center_axis',(0.,0.,-1.));
#5309=DIRECTION('ref_axis',(1.,0.,0.));
#5310=DIRECTION('',(0.,0.,-1.));
#5311=DIRECTION('center_axis',(0.,0.,1.));
#5312=DIRECTION('ref_axis',(1.,0.,0.));
#5313=DIRECTION('center_axis',(0.,0.,1.));
#5314=DIRECTION('ref_axis',(1.,0.,0.));
#5315=DIRECTION('',(0.,0.,-1.));
#5316=DIRECTION('center_axis',(0.,0.,1.));
#5317=DIRECTION('ref_axis',(1.,0.,0.));
#5318=DIRECTION('center_axis',(0.,0.,1.));
#5319=DIRECTION('ref_axis',(1.,0.,0.));
#5320=DIRECTION('center_axis',(0.,0.,1.));
#5321=DIRECTION('ref_axis',(1.,0.,0.));
#5322=DIRECTION('axis',(0.,0.,1.));
#5323=DIRECTION('refdir',(1.,0.,0.));
#5324=DIRECTION('center_axis',(0.,0.,1.));
#5325=DIRECTION('ref_axis',(1.,0.,0.));
#5326=DIRECTION('center_axis',(0.,0.,1.));
#5327=DIRECTION('ref_axis',(1.,0.,0.));
#5328=DIRECTION('',(0.,0.,1.));
#5329=DIRECTION('center_axis',(0.,0.,-1.));
#5330=DIRECTION('ref_axis',(1.,0.,0.));
#5331=DIRECTION('center_axis',(0.,0.,1.));
#5332=DIRECTION('ref_axis',(1.,0.,0.));
#5333=DIRECTION('center_axis',(0.,0.,1.));
#5334=DIRECTION('ref_axis',(1.,0.,0.));
#5335=DIRECTION('center_axis',(0.,0.,1.));
#5336=DIRECTION('ref_axis',(1.,0.,0.));
#5337=DIRECTION('',(0.,0.,1.));
#5338=DIRECTION('center_axis',(0.,0.,-1.));
#5339=DIRECTION('ref_axis',(1.,0.,0.));
#5340=DIRECTION('center_axis',(0.,0.,1.));
#5341=DIRECTION('ref_axis',(1.,0.,0.));
#5342=DIRECTION('center_axis',(0.,0.,1.));
#5343=DIRECTION('ref_axis',(1.,0.,0.));
#5344=DIRECTION('center_axis',(0.,0.,1.));
#5345=DIRECTION('ref_axis',(1.,0.,0.));
#5346=DIRECTION('',(0.,0.,1.));
#5347=DIRECTION('center_axis',(0.,0.,-1.));
#5348=DIRECTION('ref_axis',(1.,0.,0.));
#5349=DIRECTION('center_axis',(0.,0.,1.));
#5350=DIRECTION('ref_axis',(1.,0.,0.));
#5351=DIRECTION('center_axis',(0.,0.,1.));
#5352=DIRECTION('ref_axis',(1.,0.,0.));
#5353=DIRECTION('',(0.,0.,1.));
#5354=DIRECTION('center_axis',(0.,0.,-1.));
#5355=DIRECTION('ref_axis',(1.,0.,0.));
#5356=DIRECTION('center_axis',(0.,0.,1.));
#5357=DIRECTION('ref_axis',(1.,0.,0.));
#5358=DIRECTION('center_axis',(0.,0.,1.));
#5359=DIRECTION('ref_axis',(1.,0.,0.));
#5360=DIRECTION('',(0.,0.,1.));
#5361=DIRECTION('center_axis',(0.,0.,-1.));
#5362=DIRECTION('ref_axis',(1.,0.,0.));
#5363=DIRECTION('center_axis',(0.,0.,1.));
#5364=DIRECTION('ref_axis',(1.,0.,0.));
#5365=DIRECTION('center_axis',(0.,0.,1.));
#5366=DIRECTION('ref_axis',(1.,0.,0.));
#5367=DIRECTION('',(0.,0.,1.));
#5368=DIRECTION('center_axis',(0.,0.,-1.));
#5369=DIRECTION('ref_axis',(1.,0.,0.));
#5370=DIRECTION('center_axis',(0.,0.,1.));
#5371=DIRECTION('ref_axis',(1.,0.,0.));
#5372=DIRECTION('center_axis',(0.,0.,1.));
#5373=DIRECTION('ref_axis',(1.,0.,0.));
#5374=DIRECTION('',(0.,0.,1.));
#5375=DIRECTION('center_axis',(0.,0.,-1.));
#5376=DIRECTION('ref_axis',(1.,0.,0.));
#5377=DIRECTION('center_axis',(0.,1.,0.));
#5378=DIRECTION('ref_axis',(-1.,0.,0.));
#5379=DIRECTION('',(-1.,0.,0.));
#5380=DIRECTION('',(0.,0.,1.));
#5381=DIRECTION('',(-1.,0.,0.));
#5382=DIRECTION('',(0.,0.,1.));
#5383=DIRECTION('center_axis',(1.,0.,0.));
#5384=DIRECTION('ref_axis',(0.,1.,0.));
#5385=DIRECTION('',(0.,1.,0.));
#5386=DIRECTION('',(0.,1.,0.));
#5387=DIRECTION('',(0.,0.,1.));
#5388=DIRECTION('center_axis',(0.,-1.,0.));
#5389=DIRECTION('ref_axis',(1.,0.,0.));
#5390=DIRECTION('',(1.,0.,0.));
#5391=DIRECTION('',(1.,0.,0.));
#5392=DIRECTION('',(0.,0.,1.));
#5393=DIRECTION('center_axis',(-1.,0.,0.));
#5394=DIRECTION('ref_axis',(0.,-1.,0.));
#5395=DIRECTION('',(0.,-1.,0.));
#5396=DIRECTION('',(0.,-1.,0.));
#5397=DIRECTION('center_axis',(0.,0.,1.));
#5398=DIRECTION('ref_axis',(1.,0.,0.));
#5399=DIRECTION('center_axis',(0.,0.,1.));
#5400=DIRECTION('ref_axis',(1.,0.,0.));
#5401=DIRECTION('axis',(0.,0.,1.));
#5402=DIRECTION('refdir',(1.,0.,0.));
#5403=DIRECTION('center_axis',(0.,0.,1.));
#5404=DIRECTION('ref_axis',(1.,0.,0.));
#5405=DIRECTION('center_axis',(0.,0.,-1.));
#5406=DIRECTION('ref_axis',(1.,0.,0.));
#5407=DIRECTION('',(0.,0.,-1.));
#5408=DIRECTION('center_axis',(0.,0.,-1.));
#5409=DIRECTION('ref_axis',(1.,0.,0.));
#5410=DIRECTION('center_axis',(0.,0.,1.));
#5411=DIRECTION('ref_axis',(1.,0.,0.));
#5412=DIRECTION('center_axis',(0.,0.,1.));
#5413=DIRECTION('ref_axis',(1.,0.,0.));
#5414=DIRECTION('',(0.,0.,-1.));
#5415=DIRECTION('center_axis',(0.,0.,1.));
#5416=DIRECTION('ref_axis',(1.,0.,0.));
#5417=DIRECTION('center_axis',(0.,0.,1.));
#5418=DIRECTION('ref_axis',(1.,0.,0.));
#5419=DIRECTION('center_axis',(0.,0.,1.));
#5420=DIRECTION('ref_axis',(1.,0.,0.));
#5421=DIRECTION('axis',(0.,0.,1.));
#5422=DIRECTION('refdir',(1.,0.,0.));
#5423=DIRECTION('center_axis',(0.,0.,1.));
#5424=DIRECTION('ref_axis',(1.,0.,0.));
#5425=DIRECTION('center_axis',(0.,0.,-1.));
#5426=DIRECTION('ref_axis',(1.,0.,0.));
#5427=DIRECTION('',(0.,0.,-1.));
#5428=DIRECTION('center_axis',(0.,0.,-1.));
#5429=DIRECTION('ref_axis',(1.,0.,0.));
#5430=DIRECTION('center_axis',(0.,0.,1.));
#5431=DIRECTION('ref_axis',(1.,0.,0.));
#5432=DIRECTION('center_axis',(0.,0.,1.));
#5433=DIRECTION('ref_axis',(1.,0.,0.));
#5434=DIRECTION('',(0.,0.,-1.));
#5435=DIRECTION('center_axis',(0.,0.,1.));
#5436=DIRECTION('ref_axis',(1.,0.,0.));
#5437=DIRECTION('center_axis',(0.,0.,1.));
#5438=DIRECTION('ref_axis',(1.,0.,0.));
#5439=DIRECTION('center_axis',(0.,0.,1.));
#5440=DIRECTION('ref_axis',(1.,0.,0.));
#5441=DIRECTION('axis',(0.,0.,1.));
#5442=DIRECTION('refdir',(1.,0.,0.));
#5443=DIRECTION('center_axis',(0.,0.,1.));
#5444=DIRECTION('ref_axis',(1.,0.,0.));
#5445=DIRECTION('center_axis',(0.,0.,-1.));
#5446=DIRECTION('ref_axis',(1.,0.,0.));
#5447=DIRECTION('',(0.,0.,-1.));
#5448=DIRECTION('center_axis',(0.,0.,-1.));
#5449=DIRECTION('ref_axis',(1.,0.,0.));
#5450=DIRECTION('center_axis',(0.,0.,1.));
#5451=DIRECTION('ref_axis',(1.,0.,0.));
#5452=DIRECTION('center_axis',(0.,0.,1.));
#5453=DIRECTION('ref_axis',(1.,0.,0.));
#5454=DIRECTION('',(0.,0.,-1.));
#5455=DIRECTION('center_axis',(0.,0.,1.));
#5456=DIRECTION('ref_axis',(1.,0.,0.));
#5457=DIRECTION('center_axis',(0.,0.,1.));
#5458=DIRECTION('ref_axis',(1.,0.,0.));
#5459=DIRECTION('center_axis',(0.,0.,1.));
#5460=DIRECTION('ref_axis',(1.,0.,0.));
#5461=DIRECTION('axis',(0.,0.,1.));
#5462=DIRECTION('refdir',(1.,0.,0.));
#5463=DIRECTION('center_axis',(0.,0.,1.));
#5464=DIRECTION('ref_axis',(1.,0.,0.));
#5465=DIRECTION('center_axis',(0.,0.,-1.));
#5466=DIRECTION('ref_axis',(1.,0.,0.));
#5467=DIRECTION('',(0.,0.,-1.));
#5468=DIRECTION('center_axis',(0.,0.,-1.));
#5469=DIRECTION('ref_axis',(1.,0.,0.));
#5470=DIRECTION('center_axis',(0.,0.,1.));
#5471=DIRECTION('ref_axis',(1.,0.,0.));
#5472=DIRECTION('center_axis',(0.,0.,1.));
#5473=DIRECTION('ref_axis',(1.,0.,0.));
#5474=DIRECTION('',(0.,0.,-1.));
#5475=DIRECTION('center_axis',(0.,0.,1.));
#5476=DIRECTION('ref_axis',(1.,0.,0.));
#5477=DIRECTION('center_axis',(0.,0.,1.));
#5478=DIRECTION('ref_axis',(1.,0.,0.));
#5479=DIRECTION('center_axis',(0.,0.,1.));
#5480=DIRECTION('ref_axis',(1.,0.,0.));
#5481=DIRECTION('axis',(0.,0.,1.));
#5482=DIRECTION('refdir',(1.,0.,0.));
#5483=DIRECTION('center_axis',(0.,0.,1.));
#5484=DIRECTION('ref_axis',(1.,0.,0.));
#5485=DIRECTION('center_axis',(0.,0.,1.));
#5486=DIRECTION('ref_axis',(1.,0.,0.));
#5487=DIRECTION('',(0.,0.,-1.));
#5488=DIRECTION('center_axis',(0.,0.,1.));
#5489=DIRECTION('ref_axis',(1.,0.,0.));
#5490=DIRECTION('center_axis',(0.,0.,1.));
#5491=DIRECTION('ref_axis',(1.,0.,0.));
#5492=DIRECTION('center_axis',(0.,0.,1.));
#5493=DIRECTION('ref_axis',(1.,0.,0.));
#5494=DIRECTION('axis',(0.,0.,1.));
#5495=DIRECTION('refdir',(1.,0.,0.));
#5496=DIRECTION('center_axis',(0.,0.,1.));
#5497=DIRECTION('ref_axis',(1.,0.,0.));
#5498=DIRECTION('center_axis',(0.,0.,1.));
#5499=DIRECTION('ref_axis',(1.,0.,0.));
#5500=DIRECTION('',(0.,0.,-1.));
#5501=DIRECTION('center_axis',(0.,0.,1.));
#5502=DIRECTION('ref_axis',(1.,0.,0.));
#5503=DIRECTION('center_axis',(0.,0.,1.));
#5504=DIRECTION('ref_axis',(1.,0.,0.));
#5505=DIRECTION('center_axis',(0.,0.,1.));
#5506=DIRECTION('ref_axis',(1.,0.,0.));
#5507=DIRECTION('axis',(0.,0.,1.));
#5508=DIRECTION('refdir',(1.,0.,0.));
#5509=DIRECTION('center_axis',(0.866025403784439,0.,-0.5));
#5510=DIRECTION('ref_axis',(0.5,0.,0.866025403784439));
#5511=DIRECTION('',(-0.5,0.,-0.866025403784439));
#5512=DIRECTION('',(0.,-1.,0.));
#5513=DIRECTION('',(0.5,0.,0.866025403784439));
#5514=DIRECTION('',(0.,-1.,0.));
#5515=DIRECTION('center_axis',(1.20185167898973E-16,0.,-1.));
#5516=DIRECTION('ref_axis',(1.,0.,1.20185167898973E-16));
#5517=DIRECTION('',(-1.,0.,-1.20185167898973E-16));
#5518=DIRECTION('',(0.,-1.,0.));
#5519=DIRECTION('',(1.,0.,1.20185167898973E-16));
#5520=DIRECTION('center_axis',(-0.866025403784439,0.,-0.5));
#5521=DIRECTION('ref_axis',(0.5,0.,-0.866025403784439));
#5522=DIRECTION('',(-0.5,0.,0.866025403784439));
#5523=DIRECTION('',(0.,-1.,0.));
#5524=DIRECTION('',(0.5,0.,-0.866025403784439));
#5525=DIRECTION('center_axis',(-0.866025403784439,0.,0.5));
#5526=DIRECTION('ref_axis',(-0.5,0.,-0.866025403784439));
#5527=DIRECTION('',(0.5,0.,0.866025403784439));
#5528=DIRECTION('',(0.,-1.,0.));
#5529=DIRECTION('',(-0.5,0.,-0.866025403784439));
#5530=DIRECTION('center_axis',(-2.40370335797945E-16,0.,1.));
#5531=DIRECTION('ref_axis',(-1.,0.,-2.40370335797945E-16));
#5532=DIRECTION('',(1.,0.,2.40370335797945E-16));
#5533=DIRECTION('',(0.,-1.,0.));
#5534=DIRECTION('',(-1.,0.,-2.40370335797945E-16));
#5535=DIRECTION('center_axis',(0.866025403784439,0.,0.5));
#5536=DIRECTION('ref_axis',(-0.5,0.,0.866025403784439));
#5537=DIRECTION('',(0.5,0.,-0.866025403784439));
#5538=DIRECTION('',(-0.5,0.,0.866025403784439));
#5539=DIRECTION('center_axis',(0.,1.,0.));
#5540=DIRECTION('ref_axis',(1.,0.,0.));
#5541=DIRECTION('center_axis',(0.,-1.,0.));
#5542=DIRECTION('ref_axis',(0.,0.,-1.));
#5543=DIRECTION('center_axis',(0.,1.,0.));
#5544=DIRECTION('ref_axis',(1.,0.,0.));
#5545=DIRECTION('center_axis',(0.,1.,0.));
#5546=DIRECTION('ref_axis',(1.,0.,0.));
#5547=DIRECTION('center_axis',(0.,1.,0.));
#5548=DIRECTION('ref_axis',(1.,0.,0.));
#5549=DIRECTION('center_axis',(0.,1.,0.));
#5550=DIRECTION('ref_axis',(1.,0.,0.));
#5551=DIRECTION('',(0.,-1.,0.));
#5552=DIRECTION('center_axis',(0.,1.,0.));
#5553=DIRECTION('ref_axis',(1.,0.,0.));
#5554=DIRECTION('center_axis',(0.,1.,0.));
#5555=DIRECTION('ref_axis',(1.,0.,0.));
#5556=DIRECTION('center_axis',(0.,1.,0.));
#5557=DIRECTION('ref_axis',(0.,0.,1.));
#5558=DIRECTION('center_axis',(0.,-1.,0.));
#5559=DIRECTION('ref_axis',(1.,0.,0.));
#5560=DIRECTION('center_axis',(0.,-1.,0.));
#5561=DIRECTION('ref_axis',(1.,0.,0.));
#5562=DIRECTION('center_axis',(0.,-1.,0.));
#5563=DIRECTION('ref_axis',(1.,0.,0.));
#5564=DIRECTION('',(0.707106781186548,0.707106781186547,8.65956056235493E-17));
#5565=DIRECTION('center_axis',(0.,-1.,0.));
#5566=DIRECTION('ref_axis',(1.,0.,0.));
#5567=DIRECTION('center_axis',(0.,-1.,0.));
#5568=DIRECTION('ref_axis',(1.,0.,0.));
#5569=DIRECTION('',(0.,1.,0.));
#5570=DIRECTION('center_axis',(0.,1.,0.));
#5571=DIRECTION('ref_axis',(1.,0.,0.));
#5572=DIRECTION('center_axis',(0.,-1.,0.));
#5573=DIRECTION('ref_axis',(1.,0.,0.));
#5574=DIRECTION('',(-0.707106781186547,0.707106781186548,-8.65956056235493E-17));
#5575=DIRECTION('center_axis',(0.,-1.,0.));
#5576=DIRECTION('ref_axis',(0.,0.,-1.));
#5577=DIRECTION('center_axis',(0.,-1.,0.));
#5578=DIRECTION('ref_axis',(1.,0.,0.));
#5579=DIRECTION('center_axis',(0.,1.,0.));
#5580=DIRECTION('ref_axis',(1.,0.,0.));
#5581=DIRECTION('center_axis',(0.,1.,0.));
#5582=DIRECTION('ref_axis',(1.,0.,0.));
#5583=DIRECTION('',(-0.447213595499958,0.894427190999916,-5.47678698264203E-17));
#5584=DIRECTION('center_axis',(0.,-1.,0.));
#5585=DIRECTION('ref_axis',(1.,0.,0.));
#5586=DIRECTION('',(0.,1.,0.));
#5587=DIRECTION('axis',(0.,0.,1.));
#5588=DIRECTION('refdir',(1.,0.,0.));
#5589=DIRECTION('center_axis',(0.,1.,0.));
#5590=DIRECTION('ref_axis',(1.,0.,0.));
#5591=DIRECTION('center_axis',(0.,1.,0.));
#5592=DIRECTION('ref_axis',(1.,0.,0.));
#5593=DIRECTION('',(0.707106781186548,-0.707106781186547,-8.65956056235494E-17));
#5594=DIRECTION('center_axis',(0.,-1.,0.));
#5595=DIRECTION('ref_axis',(1.,0.,0.));
#5596=DIRECTION('center_axis',(0.,1.,0.));
#5597=DIRECTION('ref_axis',(1.,0.,0.));
#5598=DIRECTION('',(0.,-1.,0.));
#5599=DIRECTION('center_axis',(0.,-1.,0.));
#5600=DIRECTION('ref_axis',(1.,0.,0.));
#5601=DIRECTION('center_axis',(0.,1.,0.));
#5602=DIRECTION('ref_axis',(1.,0.,0.));
#5603=DIRECTION('center_axis',(0.,1.,0.));
#5604=DIRECTION('ref_axis',(1.,0.,0.));
#5605=DIRECTION('center_axis',(0.,1.,0.));
#5606=DIRECTION('ref_axis',(1.,0.,0.));
#5607=DIRECTION('',(0.,-1.,0.));
#5608=DIRECTION('center_axis',(0.,1.,0.));
#5609=DIRECTION('ref_axis',(1.,0.,0.));
#5610=DIRECTION('center_axis',(0.,1.,0.));
#5611=DIRECTION('ref_axis',(1.,0.,0.));
#5612=DIRECTION('axis',(0.,0.,1.));
#5613=DIRECTION('refdir',(1.,0.,0.));
#5614=DIRECTION('center_axis',(0.,1.,0.));
#5615=DIRECTION('ref_axis',(1.,0.,0.));
#5616=DIRECTION('',(0.866025403784439,-0.5,1.06057523872491E-16));
#5617=DIRECTION('center_axis',(0.,-1.,0.));
#5618=DIRECTION('ref_axis',(1.,0.,0.));
#5619=DIRECTION('center_axis',(0.,-1.,0.));
#5620=DIRECTION('ref_axis',(1.,0.,0.));
#5621=DIRECTION('center_axis',(0.,1.,0.));
#5622=DIRECTION('ref_axis',(1.,0.,0.));
#5623=DIRECTION('',(-0.866025403784439,-0.5,-1.06057523872491E-16));
#5624=DIRECTION('center_axis',(1.20185167898973E-16,0.,-1.));
#5625=DIRECTION('ref_axis',(-1.,0.,-1.20185167898973E-16));
#5626=DIRECTION('',(0.,1.,0.));
#5627=DIRECTION('',(0.,1.,0.));
#5628=DIRECTION('center_axis',(-0.866025403784439,0.,-0.5));
#5629=DIRECTION('ref_axis',(-0.5,0.,0.866025403784439));
#5630=DIRECTION('',(0.,1.,0.));
#5631=DIRECTION('center_axis',(-0.866025403784439,0.,0.5));
#5632=DIRECTION('ref_axis',(0.5,0.,0.866025403784439));
#5633=DIRECTION('',(0.,1.,0.));
#5634=DIRECTION('center_axis',(0.,1.,0.));
#5635=DIRECTION('ref_axis',(1.,0.,0.));
#5636=DIRECTION('center_axis',(0.,1.,0.));
#5637=DIRECTION('ref_axis',(1.,0.,0.));
#5638=DIRECTION('',(0.,-1.,0.));
#5639=DIRECTION('center_axis',(0.,1.,0.));
#5640=DIRECTION('ref_axis',(1.,0.,0.));
#5641=DIRECTION('center_axis',(-2.40370335797945E-16,0.,1.));
#5642=DIRECTION('ref_axis',(1.,0.,2.40370335797945E-16));
#5643=DIRECTION('',(0.,1.,0.));
#5644=DIRECTION('center_axis',(0.866025403784439,0.,-0.5));
#5645=DIRECTION('ref_axis',(-0.5,0.,-0.866025403784439));
#5646=DIRECTION('',(0.,1.,0.));
#5647=DIRECTION('center_axis',(0.866025403784439,0.,0.5));
#5648=DIRECTION('ref_axis',(0.5,0.,-0.866025403784439));
#5649=DIRECTION('center_axis',(0.,1.,0.));
#5650=DIRECTION('ref_axis',(1.,0.,0.));
#5651=DIRECTION('center_axis',(0.,1.,0.));
#5652=DIRECTION('ref_axis',(1.,0.,0.));
#5653=DIRECTION('axis',(0.,0.,1.));
#5654=DIRECTION('refdir',(1.,0.,0.));
#5655=DIRECTION('center_axis',(0.,1.,0.));
#5656=DIRECTION('ref_axis',(1.,0.,0.));
#5657=DIRECTION('',(-0.5,0.,0.866025403784439));
#5658=DIRECTION('',(-1.,0.,-2.84883360945713E-16));
#5659=DIRECTION('',(-0.5,0.,-0.866025403784439));
#5660=DIRECTION('',(0.5,0.,-0.866025403784439));
#5661=DIRECTION('',(1.,0.,0.));
#5662=DIRECTION('',(0.5,0.,0.866025403784439));
#5663=DIRECTION('center_axis',(0.,-1.,0.));
#5664=DIRECTION('ref_axis',(1.,0.,0.));
#5665=DIRECTION('center_axis',(0.,1.,0.));
#5666=DIRECTION('ref_axis',(1.,0.,0.));
#5667=DIRECTION('',(0.5,0.,-0.866025403784439));
#5668=DIRECTION('',(-0.5,0.,-0.866025403784439));
#5669=DIRECTION('',(-1.,0.,0.));
#5670=DIRECTION('',(-0.5,0.,0.866025403784439));
#5671=DIRECTION('',(0.5,0.,0.866025403784439));
#5672=DIRECTION('',(1.,0.,2.84883360945713E-16));
#5673=DIRECTION('center_axis',(0.,1.,0.));
#5674=DIRECTION('ref_axis',(1.,0.,0.));
#5675=DIRECTION('center_axis',(-2.84883360945713E-16,0.,1.));
#5676=DIRECTION('ref_axis',(1.,0.,2.84883360945713E-16));
#5677=DIRECTION('',(0.,-1.,0.));
#5678=DIRECTION('',(0.,1.,0.));
#5679=DIRECTION('center_axis',(-0.866025403784439,0.,0.5));
#5680=DIRECTION('ref_axis',(0.5,0.,0.866025403784439));
#5681=DIRECTION('',(0.,1.,0.));
#5682=DIRECTION('center_axis',(-0.866025403784439,0.,-0.5));
#5683=DIRECTION('ref_axis',(-0.5,0.,0.866025403784439));
#5684=DIRECTION('',(0.,1.,0.));
#5685=DIRECTION('center_axis',(0.,0.,-1.));
#5686=DIRECTION('ref_axis',(-1.,0.,0.));
#5687=DIRECTION('',(0.,1.,0.));
#5688=DIRECTION('center_axis',(0.866025403784439,0.,-0.5));
#5689=DIRECTION('ref_axis',(-0.5,0.,-0.866025403784439));
#5690=DIRECTION('',(0.,1.,0.));
#5691=DIRECTION('center_axis',(0.866025403784439,0.,0.5));
#5692=DIRECTION('ref_axis',(0.5,0.,-0.866025403784439));
#5693=DIRECTION('center_axis',(0.,-1.,0.));
#5694=DIRECTION('ref_axis',(1.,0.,0.));
#5695=DIRECTION('',(0.,1.,0.));
#5696=DIRECTION('center_axis',(0.,-1.,0.));
#5697=DIRECTION('ref_axis',(1.,0.,0.));
#5698=DIRECTION('center_axis',(0.,1.,0.));
#5699=DIRECTION('ref_axis',(0.,0.,1.));
#5700=DIRECTION('center_axis',(0.,-1.,0.));
#5701=DIRECTION('ref_axis',(1.,0.,0.));
#5702=DIRECTION('center_axis',(0.,-1.,0.));
#5703=DIRECTION('ref_axis',(1.,0.,0.));
#5704=DIRECTION('center_axis',(0.,-1.,0.));
#5705=DIRECTION('ref_axis',(1.,0.,0.));
#5706=DIRECTION('',(0.707106781186547,0.707106781186548,8.65956056235493E-17));
#5707=DIRECTION('center_axis',(0.,-1.,0.));
#5708=DIRECTION('ref_axis',(1.,0.,0.));
#5709=DIRECTION('center_axis',(0.,-1.,0.));
#5710=DIRECTION('ref_axis',(1.,0.,0.));
#5711=DIRECTION('',(0.,1.,0.));
#5712=DIRECTION('center_axis',(0.,1.,0.));
#5713=DIRECTION('ref_axis',(1.,0.,0.));
#5714=DIRECTION('center_axis',(0.,-1.,0.));
#5715=DIRECTION('ref_axis',(1.,0.,0.));
#5716=DIRECTION('',(-0.707106781186547,0.707106781186548,-8.65956056235493E-17));
#5717=DIRECTION('center_axis',(0.,-1.,0.));
#5718=DIRECTION('ref_axis',(0.,0.,-1.));
#5719=DIRECTION('center_axis',(0.,-1.,0.));
#5720=DIRECTION('ref_axis',(1.,0.,0.));
#5721=DIRECTION('center_axis',(0.,-1.,0.));
#5722=DIRECTION('ref_axis',(1.,0.,0.));
#5723=DIRECTION('',(0.,1.,0.));
#5724=DIRECTION('axis',(0.,0.,1.));
#5725=DIRECTION('refdir',(1.,0.,0.));
#5726=DIRECTION('center_axis',(0.,1.,0.));
#5727=DIRECTION('ref_axis',(0.,0.,1.));
#5728=DIRECTION('center_axis',(0.,-1.,0.));
#5729=DIRECTION('ref_axis',(1.,0.,0.));
#5730=DIRECTION('center_axis',(0.,-1.,0.));
#5731=DIRECTION('ref_axis',(1.,0.,0.));
#5732=DIRECTION('center_axis',(0.,-1.,0.));
#5733=DIRECTION('ref_axis',(1.,0.,0.));
#5734=DIRECTION('',(0.707106781186547,0.707106781186548,8.65956056235493E-17));
#5735=DIRECTION('center_axis',(0.,-1.,0.));
#5736=DIRECTION('ref_axis',(1.,0.,0.));
#5737=DIRECTION('center_axis',(0.,-1.,0.));
#5738=DIRECTION('ref_axis',(1.,0.,0.));
#5739=DIRECTION('',(0.,1.,0.));
#5740=DIRECTION('center_axis',(0.,1.,0.));
#5741=DIRECTION('ref_axis',(1.,0.,0.));
#5742=DIRECTION('center_axis',(0.,-1.,0.));
#5743=DIRECTION('ref_axis',(1.,0.,0.));
#5744=DIRECTION('',(-0.707106781186547,0.707106781186548,-8.65956056235493E-17));
#5745=DIRECTION('center_axis',(0.,-1.,0.));
#5746=DIRECTION('ref_axis',(0.,0.,-1.));
#5747=DIRECTION('center_axis',(0.,-1.,0.));
#5748=DIRECTION('ref_axis',(1.,0.,0.));
#5749=DIRECTION('center_axis',(0.,1.,0.));
#5750=DIRECTION('ref_axis',(1.,0.,0.));
#5751=DIRECTION('center_axis',(0.,1.,0.));
#5752=DIRECTION('ref_axis',(1.,0.,0.));
#5753=DIRECTION('',(-0.447213595499958,0.894427190999916,-5.47678698264203E-17));
#5754=DIRECTION('center_axis',(0.,-1.,0.));
#5755=DIRECTION('ref_axis',(1.,0.,0.));
#5756=DIRECTION('center_axis',(0.,1.,0.));
#5757=DIRECTION('ref_axis',(1.,0.,0.));
#5758=DIRECTION('',(0.,1.,0.));
#5759=DIRECTION('center_axis',(0.,1.,0.));
#5760=DIRECTION('ref_axis',(1.,0.,0.));
#5761=DIRECTION('center_axis',(0.,-1.,0.));
#5762=DIRECTION('ref_axis',(1.,0.,0.));
#5763=DIRECTION('',(-0.707106781186547,0.707106781186548,-8.65956056235493E-17));
#5764=DIRECTION('center_axis',(0.,-1.,0.));
#5765=DIRECTION('ref_axis',(0.,0.,-1.));
#5766=DIRECTION('center_axis',(0.866025403784439,0.,-0.5));
#5767=DIRECTION('ref_axis',(0.5,0.,0.866025403784439));
#5768=DIRECTION('',(-0.5,0.,-0.866025403784439));
#5769=DIRECTION('',(0.,-1.,0.));
#5770=DIRECTION('',(0.5,0.,0.866025403784439));
#5771=DIRECTION('',(0.,-1.,0.));
#5772=DIRECTION('center_axis',(1.60246890531964E-16,0.,-1.));
#5773=DIRECTION('ref_axis',(1.,0.,1.60246890531964E-16));
#5774=DIRECTION('',(-1.,0.,-1.60246890531964E-16));
#5775=DIRECTION('',(0.,-1.,0.));
#5776=DIRECTION('',(1.,0.,1.60246890531964E-16));
#5777=DIRECTION('center_axis',(-0.866025403784439,0.,-0.5));
#5778=DIRECTION('ref_axis',(0.5,0.,-0.866025403784439));
#5779=DIRECTION('',(-0.5,0.,0.866025403784439));
#5780=DIRECTION('',(0.,-1.,0.));
#5781=DIRECTION('',(0.5,0.,-0.866025403784439));
#5782=DIRECTION('center_axis',(-0.866025403784439,0.,0.5));
#5783=DIRECTION('ref_axis',(-0.5,0.,-0.866025403784439));
#5784=DIRECTION('',(0.5,0.,0.866025403784439));
#5785=DIRECTION('',(0.,-1.,0.));
#5786=DIRECTION('',(-0.5,0.,-0.866025403784439));
#5787=DIRECTION('center_axis',(-1.60246890531964E-16,0.,1.));
#5788=DIRECTION('ref_axis',(-1.,0.,-1.60246890531964E-16));
#5789=DIRECTION('',(1.,0.,1.60246890531964E-16));
#5790=DIRECTION('',(0.,-1.,0.));
#5791=DIRECTION('',(-1.,0.,-1.60246890531964E-16));
#5792=DIRECTION('center_axis',(0.866025403784439,0.,0.5));
#5793=DIRECTION('ref_axis',(-0.5,0.,0.866025403784439));
#5794=DIRECTION('',(0.5,0.,-0.866025403784439));
#5795=DIRECTION('',(-0.5,0.,0.866025403784439));
#5796=DIRECTION('center_axis',(0.,1.,0.));
#5797=DIRECTION('ref_axis',(1.,0.,0.));
#5798=DIRECTION('center_axis',(0.,-1.,0.));
#5799=DIRECTION('ref_axis',(0.,0.,-1.));
#5800=DIRECTION('',(0.,0.,1.));
#5801=DIRECTION('',(1.,0.,0.));
#5802=DIRECTION('',(0.,0.,1.));
#5803=DIRECTION('',(1.,0.,0.));
#5804=DIRECTION('',(0.,0.,1.));
#5805=DIRECTION('',(1.,0.,0.));
#5806=DIRECTION('',(0.,0.,1.));
#5807=DIRECTION('',(1.,0.,0.));
#5808=DIRECTION('',(0.,0.,1.));
#5809=DIRECTION('',(1.,0.,0.));
#5810=DIRECTION('',(0.,0.,1.));
#5811=DIRECTION('',(1.,0.,0.));
#5812=DIRECTION('',(0.,0.,1.));
#5813=DIRECTION('',(1.,0.,0.));
#5814=DIRECTION('',(0.,0.,1.));
#5815=DIRECTION('',(1.,0.,0.));
#5816=DIRECTION('',(0.,0.,1.));
#5817=DIRECTION('',(1.,0.,0.));
#5818=DIRECTION('',(0.,0.,1.));
#5819=DIRECTION('',(1.,0.,0.));
#5820=DIRECTION('',(0.,0.,1.));
#5821=DIRECTION('',(1.,0.,0.));
#5822=DIRECTION('',(0.,0.,1.));
#5823=DIRECTION('',(1.,0.,0.));
#5824=DIRECTION('',(0.,0.,1.));
#5825=DIRECTION('',(1.,0.,0.));
#5826=DIRECTION('',(0.,0.,1.));
#5827=DIRECTION('',(1.,0.,0.));
#5828=DIRECTION('',(0.,0.,1.));
#5829=DIRECTION('',(1.,0.,0.));
#5830=DIRECTION('',(0.,0.,1.));
#5831=DIRECTION('',(-1.,1.22464679914735E-16,0.));
#5832=DIRECTION('',(0.,0.,1.));
#5833=DIRECTION('',(-1.,1.22464679914735E-16,0.));
#5834=DIRECTION('',(0.,0.,1.));
#5835=DIRECTION('',(1.,0.,0.));
#5836=DIRECTION('',(0.,0.,1.));
#5837=DIRECTION('',(1.,0.,0.));
#5838=DIRECTION('',(0.,0.,1.));
#5839=DIRECTION('',(-1.,1.22464679914735E-16,0.));
#5840=DIRECTION('',(0.,0.,1.));
#5841=DIRECTION('',(-1.,1.22464679914735E-16,0.));
#5842=DIRECTION('',(0.,0.,1.));
#5843=DIRECTION('',(1.,0.,0.));
#5844=DIRECTION('',(0.,0.,1.));
#5845=DIRECTION('',(1.,0.,0.));
#5846=DIRECTION('',(0.,0.,1.));
#5847=DIRECTION('',(-1.,1.22464679914735E-16,0.));
#5848=DIRECTION('',(0.,0.,1.));
#5849=DIRECTION('',(-1.,1.22464679914735E-16,0.));
#5850=DIRECTION('',(0.,0.,1.));
#5851=DIRECTION('',(1.,0.,0.));
#5852=DIRECTION('',(0.,0.,1.));
#5853=DIRECTION('',(1.,0.,0.));
#5854=DIRECTION('',(0.,0.,1.));
#5855=DIRECTION('',(-1.,1.22464679914735E-16,0.));
#5856=DIRECTION('',(0.,0.,1.));
#5857=DIRECTION('',(-1.,1.22464679914735E-16,0.));
#5858=DIRECTION('',(0.,0.,1.));
#5859=DIRECTION('',(1.,0.,0.));
#5860=DIRECTION('',(0.,0.,1.));
#5861=DIRECTION('',(1.,0.,0.));
#5862=DIRECTION('',(0.,0.,1.));
#5863=DIRECTION('',(1.,0.,0.));
#5864=DIRECTION('',(0.,0.,1.));
#5865=DIRECTION('',(1.,0.,0.));
#5866=DIRECTION('',(0.,-1.,2.22044604925031E-16));
#5867=DIRECTION('',(1.,0.,0.));
#5868=DIRECTION('',(0.,-1.,2.22044604925031E-16));
#5869=DIRECTION('',(1.,0.,0.));
#5870=DIRECTION('',(0.,-1.,2.22044604925031E-16));
#5871=DIRECTION('',(1.,0.,0.));
#5872=DIRECTION('',(0.,-1.,2.22044604925031E-16));
#5873=DIRECTION('',(1.,0.,0.));
#5874=DIRECTION('axis',(0.,0.,1.));
#5875=DIRECTION('refdir',(1.,0.,0.));
#5876=DIRECTION('axis',(0.,0.,1.));
#5877=DIRECTION('refdir',(1.,0.,0.));
#5878=DIRECTION('center_axis',(0.,-1.,0.));
#5879=DIRECTION('ref_axis',(1.,0.,0.));
#5880=DIRECTION('center_axis',(0.,-1.,0.));
#5881=DIRECTION('ref_axis',(0.,0.,1.));
#5882=DIRECTION('',(0.,0.,1.));
#5883=DIRECTION('',(1.,0.,0.));
#5884=DIRECTION('',(0.,0.,1.));
#5885=DIRECTION('center_axis',(-1.,0.,0.));
#5886=DIRECTION('ref_axis',(0.,-1.,0.));
#5887=DIRECTION('center_axis',(-1.,0.,0.));
#5888=DIRECTION('ref_axis',(0.,0.,-1.));
#5889=DIRECTION('',(0.,-1.,0.));
#5890=DIRECTION('',(0.,0.,1.));
#5891=DIRECTION('center_axis',(-1.,0.,0.));
#5892=DIRECTION('ref_axis',(0.,0.,-1.));
#5893=DIRECTION('center_axis',(0.,1.,0.));
#5894=DIRECTION('ref_axis',(-1.,0.,0.));
#5895=DIRECTION('center_axis',(0.,1.,0.));
#5896=DIRECTION('ref_axis',(0.,0.,-1.));
#5897=DIRECTION('',(-1.,0.,0.));
#5898=DIRECTION('',(0.,0.,1.));
#5899=DIRECTION('center_axis',(1.,0.,0.));
#5900=DIRECTION('ref_axis',(0.,1.,0.));
#5901=DIRECTION('center_axis',(1.,0.,0.));
#5902=DIRECTION('ref_axis',(0.,0.,1.));
#5903=DIRECTION('',(0.,1.,0.));
#5904=DIRECTION('center_axis',(0.,0.,1.));
#5905=DIRECTION('ref_axis',(1.,0.,0.));
#5906=DIRECTION('center_axis',(0.,1.,0.));
#5907=DIRECTION('ref_axis',(1.,0.,0.));
#5908=DIRECTION('center_axis',(0.,1.,0.));
#5909=DIRECTION('ref_axis',(1.,0.,0.));
#5910=DIRECTION('',(0.,1.,0.));
#5911=DIRECTION('center_axis',(0.,-1.,0.));
#5912=DIRECTION('ref_axis',(1.,0.,0.));
#5913=DIRECTION('center_axis',(6.12323399573677E-17,0.,1.));
#5914=DIRECTION('ref_axis',(1.,0.,0.));
#5915=DIRECTION('center_axis',(1.22464679914735E-16,-1.,0.));
#5916=DIRECTION('ref_axis',(-1.,-1.22464679914735E-16,0.));
#5917=DIRECTION('axis',(0.,0.,1.));
#5918=DIRECTION('refdir',(1.,0.,0.));
#5919=DIRECTION('center_axis',(0.,0.,1.));
#5920=DIRECTION('ref_axis',(1.,0.,0.));
#5921=DIRECTION('center_axis',(0.,0.,1.));
#5922=DIRECTION('ref_axis',(1.,0.,0.));
#5923=DIRECTION('',(0.,0.,1.));
#5924=DIRECTION('center_axis',(0.,0.,-1.));
#5925=DIRECTION('ref_axis',(1.,0.,0.));
#5926=DIRECTION('center_axis',(0.,0.,1.));
#5927=DIRECTION('ref_axis',(1.,0.,0.));
#5928=DIRECTION('center_axis',(0.,0.,1.));
#5929=DIRECTION('ref_axis',(1.,0.,0.));
#5930=DIRECTION('center_axis',(0.,0.,1.));
#5931=DIRECTION('ref_axis',(1.,0.,0.));
#5932=DIRECTION('',(0.,-1.,0.));
#5933=DIRECTION('',(-1.,0.,0.));
#5934=DIRECTION('center_axis',(0.,0.,1.));
#5935=DIRECTION('ref_axis',(1.,0.,0.));
#5936=DIRECTION('center_axis',(0.,0.,1.));
#5937=DIRECTION('ref_axis',(1.,0.,0.));
#5938=DIRECTION('',(1.,0.,0.));
#5939=DIRECTION('',(0.,-1.,0.));
#5940=DIRECTION('center_axis',(0.,0.,1.));
#5941=DIRECTION('ref_axis',(1.,0.,0.));
#5942=DIRECTION('center_axis',(0.,0.,1.));
#5943=DIRECTION('ref_axis',(1.,0.,0.));
#5944=DIRECTION('',(0.,1.,0.));
#5945=DIRECTION('',(1.,0.,0.));
#5946=DIRECTION('center_axis',(0.,0.,1.));
#5947=DIRECTION('ref_axis',(1.,0.,0.));
#5948=DIRECTION('center_axis',(0.,0.,1.));
#5949=DIRECTION('ref_axis',(1.,0.,0.));
#5950=DIRECTION('',(-1.,0.,0.));
#5951=DIRECTION('',(0.,1.,0.));
#5952=DIRECTION('center_axis',(0.,1.,0.));
#5953=DIRECTION('ref_axis',(-1.,0.,0.));
#5954=DIRECTION('',(1.,0.,0.));
#5955=DIRECTION('',(0.,0.,1.));
#5956=DIRECTION('',(-1.,0.,0.));
#5957=DIRECTION('',(0.,0.,1.));
#5958=DIRECTION('center_axis',(1.,0.,0.));
#5959=DIRECTION('ref_axis',(0.,1.,0.));
#5960=DIRECTION('',(0.,-1.,0.));
#5961=DIRECTION('',(0.,1.,0.));
#5962=DIRECTION('',(0.,0.,1.));
#5963=DIRECTION('center_axis',(0.,-1.,0.));
#5964=DIRECTION('ref_axis',(1.,0.,0.));
#5965=DIRECTION('',(-1.,0.,0.));
#5966=DIRECTION('',(1.,0.,0.));
#5967=DIRECTION('',(0.,0.,1.));
#5968=DIRECTION('center_axis',(-1.,0.,0.));
#5969=DIRECTION('ref_axis',(0.,-1.,0.));
#5970=DIRECTION('',(0.,1.,0.));
#5971=DIRECTION('',(0.,-1.,0.));
#5972=DIRECTION('center_axis',(0.,0.,1.));
#5973=DIRECTION('ref_axis',(1.,0.,0.));
#5974=DIRECTION('center_axis',(0.,0.,1.));
#5975=DIRECTION('ref_axis',(1.,0.,0.));
#5976=DIRECTION('center_axis',(0.,0.,1.));
#5977=DIRECTION('ref_axis',(1.,0.,0.));
#5978=DIRECTION('center_axis',(0.,0.,1.));
#5979=DIRECTION('ref_axis',(1.,0.,0.));
#5980=DIRECTION('center_axis',(0.,0.,1.));
#5981=DIRECTION('ref_axis',(1.,0.,0.));
#5982=DIRECTION('center_axis',(0.,0.,1.));
#5983=DIRECTION('ref_axis',(1.,0.,0.));
#5984=DIRECTION('center_axis',(0.,0.,1.));
#5985=DIRECTION('ref_axis',(1.,0.,0.));
#5986=DIRECTION('center_axis',(0.,0.,1.));
#5987=DIRECTION('ref_axis',(1.,0.,0.));
#5988=DIRECTION('center_axis',(0.,0.,1.));
#5989=DIRECTION('ref_axis',(1.,0.,0.));
#5990=DIRECTION('center_axis',(0.,0.,1.));
#5991=DIRECTION('ref_axis',(1.,0.,0.));
#5992=DIRECTION('center_axis',(0.,1.,0.));
#5993=DIRECTION('ref_axis',(-1.,0.,0.));
#5994=DIRECTION('',(-1.,0.,0.));
#5995=DIRECTION('',(0.,0.,1.));
#5996=DIRECTION('',(-1.,0.,0.));
#5997=DIRECTION('',(0.,0.,1.));
#5998=DIRECTION('center_axis',(1.,0.,0.));
#5999=DIRECTION('ref_axis',(0.,1.,0.));
#6000=DIRECTION('',(0.,1.,0.));
#6001=DIRECTION('',(0.,1.,0.));
#6002=DIRECTION('',(0.,0.,1.));
#6003=DIRECTION('center_axis',(0.,-1.,0.));
#6004=DIRECTION('ref_axis',(1.,0.,0.));
#6005=DIRECTION('',(1.,0.,0.));
#6006=DIRECTION('',(1.,0.,0.));
#6007=DIRECTION('',(0.,0.,1.));
#6008=DIRECTION('center_axis',(-1.,0.,0.));
#6009=DIRECTION('ref_axis',(0.,-1.,0.));
#6010=DIRECTION('',(0.,-1.,0.));
#6011=DIRECTION('',(0.,-1.,0.));
#6012=DIRECTION('center_axis',(0.,0.,1.));
#6013=DIRECTION('ref_axis',(1.,0.,0.));
#6014=DIRECTION('center_axis',(0.,0.,1.));
#6015=DIRECTION('ref_axis',(1.,0.,0.));
#6016=DIRECTION('',(0.,0.,-1.));
#6017=DIRECTION('center_axis',(0.,0.,1.));
#6018=DIRECTION('ref_axis',(1.,0.,0.));
#6019=DIRECTION('center_axis',(0.,0.,1.));
#6020=DIRECTION('ref_axis',(1.,0.,0.));
#6021=DIRECTION('axis',(0.,0.,1.));
#6022=DIRECTION('refdir',(1.,0.,0.));
#6023=DIRECTION('center_axis',(0.,-1.,0.));
#6024=DIRECTION('ref_axis',(1.,0.,0.));
#6025=DIRECTION('',(-1.,0.,0.));
#6026=DIRECTION('',(0.,0.,1.));
#6027=DIRECTION('',(1.,0.,0.));
#6028=DIRECTION('',(0.,0.,1.));
#6029=DIRECTION('center_axis',(-1.,0.,0.));
#6030=DIRECTION('ref_axis',(0.,-1.,0.));
#6031=DIRECTION('',(0.,1.,0.));
#6032=DIRECTION('',(0.,-1.,0.));
#6033=DIRECTION('',(0.,0.,1.));
#6034=DIRECTION('center_axis',(0.,1.,0.));
#6035=DIRECTION('ref_axis',(-1.,0.,0.));
#6036=DIRECTION('',(1.,0.,0.));
#6037=DIRECTION('',(-1.,0.,0.));
#6038=DIRECTION('',(0.,0.,1.));
#6039=DIRECTION('center_axis',(1.,0.,0.));
#6040=DIRECTION('ref_axis',(0.,1.,0.));
#6041=DIRECTION('',(0.,-1.,0.));
#6042=DIRECTION('',(0.,1.,0.));
#6043=DIRECTION('center_axis',(0.,1.,0.));
#6044=DIRECTION('ref_axis',(-1.,0.,0.));
#6045=DIRECTION('',(-1.,0.,0.));
#6046=DIRECTION('',(0.,0.,1.));
#6047=DIRECTION('',(-1.,0.,0.));
#6048=DIRECTION('',(0.,0.,1.));
#6049=DIRECTION('center_axis',(1.,0.,0.));
#6050=DIRECTION('ref_axis',(0.,1.,0.));
#6051=DIRECTION('',(0.,1.,0.));
#6052=DIRECTION('',(0.,1.,0.));
#6053=DIRECTION('',(0.,0.,1.));
#6054=DIRECTION('center_axis',(0.,-1.,0.));
#6055=DIRECTION('ref_axis',(1.,0.,0.));
#6056=DIRECTION('',(1.,0.,0.));
#6057=DIRECTION('',(1.,0.,0.));
#6058=DIRECTION('',(0.,0.,1.));
#6059=DIRECTION('center_axis',(-1.,0.,0.));
#6060=DIRECTION('ref_axis',(0.,-1.,0.));
#6061=DIRECTION('',(0.,-1.,0.));
#6062=DIRECTION('',(0.,-1.,0.));
#6063=DIRECTION('center_axis',(0.,0.,1.));
#6064=DIRECTION('ref_axis',(1.,0.,0.));
#6065=DIRECTION('center_axis',(0.,0.,1.));
#6066=DIRECTION('ref_axis',(1.,0.,0.));
#6067=DIRECTION('axis',(0.,0.,1.));
#6068=DIRECTION('refdir',(1.,0.,0.));
#6069=DIRECTION('center_axis',(0.,0.,1.));
#6070=DIRECTION('ref_axis',(1.,0.,0.));
#6071=DIRECTION('center_axis',(0.,0.,-1.));
#6072=DIRECTION('ref_axis',(1.,0.,0.));
#6073=DIRECTION('',(0.,0.,-1.));
#6074=DIRECTION('center_axis',(0.,0.,-1.));
#6075=DIRECTION('ref_axis',(1.,0.,0.));
#6076=DIRECTION('center_axis',(0.,0.,1.));
#6077=DIRECTION('ref_axis',(1.,0.,0.));
#6078=DIRECTION('center_axis',(0.,0.,1.));
#6079=DIRECTION('ref_axis',(1.,0.,0.));
#6080=DIRECTION('',(0.,0.,-1.));
#6081=DIRECTION('center_axis',(0.,0.,1.));
#6082=DIRECTION('ref_axis',(1.,0.,0.));
#6083=DIRECTION('center_axis',(0.,0.,1.));
#6084=DIRECTION('ref_axis',(1.,0.,0.));
#6085=DIRECTION('center_axis',(0.,0.,1.));
#6086=DIRECTION('ref_axis',(1.,0.,0.));
#6087=DIRECTION('axis',(0.,0.,1.));
#6088=DIRECTION('refdir',(1.,0.,0.));
#6089=DIRECTION('center_axis',(0.,1.,0.));
#6090=DIRECTION('ref_axis',(-1.,0.,0.));
#6091=DIRECTION('',(-1.,0.,0.));
#6092=DIRECTION('',(0.,0.,1.));
#6093=DIRECTION('',(-1.,0.,0.));
#6094=DIRECTION('',(0.,0.,1.));
#6095=DIRECTION('center_axis',(1.,0.,0.));
#6096=DIRECTION('ref_axis',(0.,1.,0.));
#6097=DIRECTION('',(0.,1.,0.));
#6098=DIRECTION('',(0.,1.,0.));
#6099=DIRECTION('',(0.,0.,1.));
#6100=DIRECTION('center_axis',(0.,-1.,0.));
#6101=DIRECTION('ref_axis',(1.,0.,0.));
#6102=DIRECTION('',(1.,0.,0.));
#6103=DIRECTION('',(1.,0.,0.));
#6104=DIRECTION('',(0.,0.,1.));
#6105=DIRECTION('center_axis',(-1.,0.,0.));
#6106=DIRECTION('ref_axis',(0.,-1.,0.));
#6107=DIRECTION('',(0.,-1.,0.));
#6108=DIRECTION('',(0.,-1.,0.));
#6109=DIRECTION('center_axis',(0.,0.,1.));
#6110=DIRECTION('ref_axis',(1.,0.,0.));
#6111=DIRECTION('center_axis',(0.,0.,1.));
#6112=DIRECTION('ref_axis',(1.,0.,0.));
#6113=DIRECTION('axis',(0.,0.,1.));
#6114=DIRECTION('refdir',(1.,0.,0.));
#6115=DIRECTION('center_axis',(0.866025403784439,0.,-0.5));
#6116=DIRECTION('ref_axis',(0.5,0.,0.866025403784439));
#6117=DIRECTION('',(-0.5,0.,-0.866025403784439));
#6118=DIRECTION('',(0.,-1.,0.));
#6119=DIRECTION('',(0.5,0.,0.866025403784439));
#6120=DIRECTION('',(0.,-1.,0.));
#6121=DIRECTION('center_axis',(1.60246890531964E-16,0.,-1.));
#6122=DIRECTION('ref_axis',(1.,0.,1.60246890531964E-16));
#6123=DIRECTION('',(-1.,0.,-1.60246890531964E-16));
#6124=DIRECTION('',(0.,-1.,0.));
#6125=DIRECTION('',(1.,0.,1.60246890531964E-16));
#6126=DIRECTION('center_axis',(-0.866025403784439,0.,-0.5));
#6127=DIRECTION('ref_axis',(0.5,0.,-0.866025403784439));
#6128=DIRECTION('',(-0.5,0.,0.866025403784439));
#6129=DIRECTION('',(0.,-1.,0.));
#6130=DIRECTION('',(0.5,0.,-0.866025403784439));
#6131=DIRECTION('center_axis',(-0.866025403784439,0.,0.5));
#6132=DIRECTION('ref_axis',(-0.5,0.,-0.866025403784439));
#6133=DIRECTION('',(0.5,0.,0.866025403784439));
#6134=DIRECTION('',(0.,-1.,0.));
#6135=DIRECTION('',(-0.5,0.,-0.866025403784439));
#6136=DIRECTION('center_axis',(-1.60246890531964E-16,0.,1.));
#6137=DIRECTION('ref_axis',(-1.,0.,-1.60246890531964E-16));
#6138=DIRECTION('',(1.,0.,1.60246890531964E-16));
#6139=DIRECTION('',(0.,-1.,0.));
#6140=DIRECTION('',(-1.,0.,-1.60246890531964E-16));
#6141=DIRECTION('center_axis',(0.866025403784439,0.,0.5));
#6142=DIRECTION('ref_axis',(-0.5,0.,0.866025403784439));
#6143=DIRECTION('',(0.5,0.,-0.866025403784439));
#6144=DIRECTION('',(-0.5,0.,0.866025403784439));
#6145=DIRECTION('center_axis',(0.,1.,0.));
#6146=DIRECTION('ref_axis',(1.,0.,0.));
#6147=DIRECTION('center_axis',(0.,-1.,0.));
#6148=DIRECTION('ref_axis',(0.,0.,-1.));
#6149=DIRECTION('center_axis',(0.,1.,0.));
#6150=DIRECTION('ref_axis',(1.,0.,0.));
#6151=DIRECTION('center_axis',(0.,1.,0.));
#6152=DIRECTION('ref_axis',(1.,0.,0.));
#6153=DIRECTION('center_axis',(0.,1.,0.));
#6154=DIRECTION('ref_axis',(0.,0.,1.));
#6155=DIRECTION('center_axis',(0.,-1.,0.));
#6156=DIRECTION('ref_axis',(1.,0.,0.));
#6157=DIRECTION('center_axis',(0.,-1.,0.));
#6158=DIRECTION('ref_axis',(1.,0.,0.));
#6159=DIRECTION('center_axis',(0.,-1.,0.));
#6160=DIRECTION('ref_axis',(1.,0.,0.));
#6161=DIRECTION('',(0.707106781186547,0.707106781186548,8.65956056235493E-17));
#6162=DIRECTION('center_axis',(0.,-1.,0.));
#6163=DIRECTION('ref_axis',(1.,0.,0.));
#6164=DIRECTION('center_axis',(0.,-1.,0.));
#6165=DIRECTION('ref_axis',(1.,0.,0.));
#6166=DIRECTION('',(0.,1.,0.));
#6167=DIRECTION('center_axis',(0.,1.,0.));
#6168=DIRECTION('ref_axis',(1.,0.,0.));
#6169=DIRECTION('center_axis',(0.,-1.,0.));
#6170=DIRECTION('ref_axis',(1.,0.,0.));
#6171=DIRECTION('',(-0.707106781186547,0.707106781186548,-8.65956056235493E-17));
#6172=DIRECTION('center_axis',(0.,-1.,0.));
#6173=DIRECTION('ref_axis',(0.,0.,-1.));
#6174=DIRECTION('center_axis',(0.,-1.,0.));
#6175=DIRECTION('ref_axis',(1.,0.,0.));
#6176=DIRECTION('center_axis',(0.,1.,0.));
#6177=DIRECTION('ref_axis',(1.,0.,0.));
#6178=DIRECTION('center_axis',(0.,1.,0.));
#6179=DIRECTION('ref_axis',(1.,0.,0.));
#6180=DIRECTION('',(-0.447213595499958,0.894427190999916,-5.47678698264203E-17));
#6181=DIRECTION('center_axis',(0.,-1.,0.));
#6182=DIRECTION('ref_axis',(1.,0.,0.));
#6183=DIRECTION('',(0.,1.,0.));
#6184=DIRECTION('',(0.,0.,1.));
#6185=DIRECTION('',(1.,0.,0.));
#6186=DIRECTION('',(0.,0.,1.));
#6187=DIRECTION('',(1.,0.,0.));
#6188=DIRECTION('',(0.,0.,1.));
#6189=DIRECTION('',(1.,0.,0.));
#6190=DIRECTION('',(0.,0.,1.));
#6191=DIRECTION('',(1.,0.,0.));
#6192=DIRECTION('',(0.,0.,1.));
#6193=DIRECTION('',(1.,0.,0.));
#6194=DIRECTION('',(0.,-1.,2.22044604925031E-16));
#6195=DIRECTION('',(1.,0.,0.));
#6196=DIRECTION('',(0.,0.,1.));
#6197=DIRECTION('',(1.,0.,0.));
#6198=DIRECTION('',(0.,0.,1.));
#6199=DIRECTION('',(1.,0.,0.));
#6200=CARTESIAN_POINT('',(0.,0.,0.));
#6201=CARTESIAN_POINT('',(0.,0.,0.));
#6202=CARTESIAN_POINT('',(0.,0.,0.));
#6203=CARTESIAN_POINT('Origin',(-1.3,-1.,6.8));
#6204=CARTESIAN_POINT('',(-1.465,-1.,6.8));
#6205=CARTESIAN_POINT('Origin',(-1.3,-1.,6.8));
#6206=CARTESIAN_POINT('',(-1.465,-1.,7.5));
#6207=CARTESIAN_POINT('',(-1.465,-1.,6.8));
#6208=CARTESIAN_POINT('Origin',(-1.3,-1.,7.5));
#6209=CARTESIAN_POINT('Origin',(-1.3,-1.,6.8));
#6210=CARTESIAN_POINT('Origin',(1.3,-1.,6.8));
#6211=CARTESIAN_POINT('',(1.135,-1.,6.8));
#6212=CARTESIAN_POINT('Origin',(1.3,-1.,6.8));
#6213=CARTESIAN_POINT('',(1.135,-1.,7.5));
#6214=CARTESIAN_POINT('',(1.135,-1.,6.8));
#6215=CARTESIAN_POINT('Origin',(1.3,-1.,7.5));
#6216=CARTESIAN_POINT('Origin',(1.3,-1.,6.8));
#6217=CARTESIAN_POINT('Origin',(1.9,-3.1,3.1));
#6218=CARTESIAN_POINT('',(1.625,-3.,3.1));
#6219=CARTESIAN_POINT('Origin',(1.9,-3.,3.1));
#6220=CARTESIAN_POINT('',(1.625,-0.0249999999999999,3.1));
#6221=CARTESIAN_POINT('',(1.625,-3.1,3.1));
#6222=CARTESIAN_POINT('Origin',(1.9,-0.0249999999999999,3.1));
#6223=CARTESIAN_POINT('Origin',(-1.9,-3.1,6.9));
#6224=CARTESIAN_POINT('',(-2.175,-3.,6.9));
#6225=CARTESIAN_POINT('Origin',(-1.9,-3.,6.9));
#6226=CARTESIAN_POINT('',(-2.175,-0.0249999999999999,6.9));
#6227=CARTESIAN_POINT('',(-2.175,-3.1,6.9));
#6228=CARTESIAN_POINT('Origin',(-1.9,-0.0249999999999999,6.9));
#6229=CARTESIAN_POINT('Origin',(-1.9,-3.1,3.1));
#6230=CARTESIAN_POINT('',(-2.175,-3.,3.1));
#6231=CARTESIAN_POINT('Origin',(-1.9,-3.,3.1));
#6232=CARTESIAN_POINT('',(-2.175,-0.0249999999999999,3.1));
#6233=CARTESIAN_POINT('',(-2.175,-3.1,3.1));
#6234=CARTESIAN_POINT('Origin',(-1.9,-0.0249999999999999,3.1));
#6235=CARTESIAN_POINT('Origin',(1.9,-3.1,6.9));
#6236=CARTESIAN_POINT('',(1.625,-3.,6.9));
#6237=CARTESIAN_POINT('Origin',(1.9,-3.,6.9));
#6238=CARTESIAN_POINT('',(1.625,-0.0249999999999999,6.9));
#6239=CARTESIAN_POINT('',(1.625,-3.1,6.9));
#6240=CARTESIAN_POINT('Origin',(1.9,-0.0249999999999999,6.9));
#6241=CARTESIAN_POINT('Origin',(0.,0.,6.5));
#6242=CARTESIAN_POINT('',(0.699553428981661,-0.025,6.5));
#6243=CARTESIAN_POINT('',(0.699553428981661,-0.025,7.5));
#6244=CARTESIAN_POINT('',(0.699553428981661,-0.025,6.5));
#6245=CARTESIAN_POINT('',(-0.699553428981661,-0.025,6.5));
#6246=CARTESIAN_POINT('Origin',(0.,0.,6.5));
#6247=CARTESIAN_POINT('',(-0.699553428981661,-0.025,7.5));
#6248=CARTESIAN_POINT('',(-0.699553428981661,-0.025,6.5));
#6249=CARTESIAN_POINT('Origin',(0.,0.,7.5));
#6250=CARTESIAN_POINT('Origin',(0.,0.,6.5));
#6251=CARTESIAN_POINT('',(0.556214886532175,-0.025,6.5));
#6252=CARTESIAN_POINT('',(1.25,-0.025,6.5));
#6253=CARTESIAN_POINT('',(-0.556214886532175,-0.025,6.5));
#6254=CARTESIAN_POINT('Origin',(0.,0.,6.5));
#6255=CARTESIAN_POINT('',(1.25,-0.025,6.5));
#6256=CARTESIAN_POINT('Origin',(0.,-1.5125,7.5));
#6257=CARTESIAN_POINT('',(-2.5,-0.025,7.5));
#6258=CARTESIAN_POINT('',(2.5,-0.025,7.5));
#6259=CARTESIAN_POINT('',(-2.5,-3.,7.5));
#6260=CARTESIAN_POINT('',(-2.5,-0.025,7.5));
#6261=CARTESIAN_POINT('',(2.5,-3.,7.5));
#6262=CARTESIAN_POINT('',(-2.5,-3.,7.5));
#6263=CARTESIAN_POINT('',(2.5,-0.025,7.5));
#6264=CARTESIAN_POINT('',(2.5,-3.,7.5));
#6265=CARTESIAN_POINT('',(2.5,-0.025,7.5));
#6266=CARTESIAN_POINT('Origin',(0.,-3.1,5.));
#6267=CARTESIAN_POINT('',(-0.93,-3.,5.));
#6268=CARTESIAN_POINT('Origin',(0.,-3.,5.));
#6269=CARTESIAN_POINT('',(-0.93,-1.8,5.));
#6270=CARTESIAN_POINT('',(-0.93,-3.1,5.));
#6271=CARTESIAN_POINT('Origin',(0.,-1.8,5.));
#6272=CARTESIAN_POINT('Origin',(0.,-1.8,5.));
#6273=CARTESIAN_POINT('',(-1.3,-1.8,5.));
#6274=CARTESIAN_POINT('Origin',(0.,-1.8,5.));
#6275=CARTESIAN_POINT('',(-1.3,-1.,5.));
#6276=CARTESIAN_POINT('',(-1.3,-1.8,5.));
#6277=CARTESIAN_POINT('Origin',(0.,-1.,5.));
#6278=CARTESIAN_POINT('Origin',(0.,-1.,5.));
#6279=CARTESIAN_POINT('',(-1.52958336188405E-16,-1.,6.24899959967968));
#6280=CARTESIAN_POINT('Origin',(0.,-1.,5.));
#6281=CARTESIAN_POINT('Origin',(0.,-1.8,5.));
#6282=CARTESIAN_POINT('Origin',(0.,0.,5.));
#6283=CARTESIAN_POINT('Origin',(0.,-0.025,5.));
#6284=CARTESIAN_POINT('Origin',(2.5,-0.025,2.5));
#6285=CARTESIAN_POINT('',(2.5,-0.025,2.5));
#6286=CARTESIAN_POINT('',(2.5,-0.025,2.5));
#6287=CARTESIAN_POINT('',(-2.5,-0.025,2.5));
#6288=CARTESIAN_POINT('',(2.5,-0.025,2.5));
#6289=CARTESIAN_POINT('',(-2.5,-0.025,2.5));
#6290=CARTESIAN_POINT('Origin',(2.5,-3.,2.5));
#6291=CARTESIAN_POINT('',(2.5,-3.,2.5));
#6292=CARTESIAN_POINT('',(2.5,-3.,2.5));
#6293=CARTESIAN_POINT('',(2.5,-3.,2.5));
#6294=CARTESIAN_POINT('Origin',(-2.5,-3.,2.5));
#6295=CARTESIAN_POINT('',(-2.5,-3.,2.5));
#6296=CARTESIAN_POINT('',(-2.5,-3.,2.5));
#6297=CARTESIAN_POINT('',(-2.5,-3.,2.5));
#6298=CARTESIAN_POINT('Origin',(-2.5,-0.025,2.5));
#6299=CARTESIAN_POINT('',(-2.5,-0.025,2.5));
#6300=CARTESIAN_POINT('Origin',(0.,-1.5125,2.5));
#6301=CARTESIAN_POINT('',(0.,0.,0.));
#6302=CARTESIAN_POINT('Origin',(0.,0.,5.));
#6303=CARTESIAN_POINT('',(-1.36919674566051E-16,-1.,6.11803398874989));
#6304=CARTESIAN_POINT('Origin',(0.,-1.,5.));
#6305=CARTESIAN_POINT('',(-0.75,-1.29903810567666,5.));
#6306=CARTESIAN_POINT('Origin',(0.,-1.29903810567666,5.));
#6307=CARTESIAN_POINT('Origin',(0.,-1.8,5.));
#6308=CARTESIAN_POINT('',(-0.75,-1.8,5.));
#6309=CARTESIAN_POINT('',(-0.75,-1.8,5.));
#6310=CARTESIAN_POINT('Origin',(0.,-1.8,5.));
#6311=CARTESIAN_POINT('Origin',(0.,-1.8,5.));
#6312=CARTESIAN_POINT('',(-1.3,-1.,5.));
#6313=CARTESIAN_POINT('Origin',(0.,-1.,5.));
#6314=CARTESIAN_POINT('',(-1.3,-1.8,5.));
#6315=CARTESIAN_POINT('',(-1.3,-1.8,5.));
#6316=CARTESIAN_POINT('Origin',(0.,-1.8,5.));
#6317=CARTESIAN_POINT('Origin',(0.,-1.,5.));
#6318=CARTESIAN_POINT('Origin',(0.,-1.8,5.));
#6319=CARTESIAN_POINT('',(0.,0.,0.));
#6320=CARTESIAN_POINT('Origin',(-1.3,1.,6.8));
#6321=CARTESIAN_POINT('',(-1.465,1.,6.8));
#6322=CARTESIAN_POINT('Origin',(-1.3,1.,6.8));
#6323=CARTESIAN_POINT('',(-1.465,1.,7.5));
#6324=CARTESIAN_POINT('',(-1.465,1.,6.8));
#6325=CARTESIAN_POINT('Origin',(-1.3,1.,7.5));
#6326=CARTESIAN_POINT('Origin',(-1.3,1.,6.8));
#6327=CARTESIAN_POINT('Origin',(1.3,1.,6.8));
#6328=CARTESIAN_POINT('',(1.135,1.,6.8));
#6329=CARTESIAN_POINT('Origin',(1.3,1.,6.8));
#6330=CARTESIAN_POINT('',(1.135,1.,7.5));
#6331=CARTESIAN_POINT('',(1.135,1.,6.8));
#6332=CARTESIAN_POINT('Origin',(1.3,1.,7.5));
#6333=CARTESIAN_POINT('Origin',(1.3,1.,6.8));
#6334=CARTESIAN_POINT('Origin',(1.9,-3.1,3.1));
#6335=CARTESIAN_POINT('',(1.625,0.0249999999999999,3.1));
#6336=CARTESIAN_POINT('Origin',(1.9,0.0249999999999999,3.1));
#6337=CARTESIAN_POINT('',(1.625,3.,3.1));
#6338=CARTESIAN_POINT('',(1.625,-3.1,3.1));
#6339=CARTESIAN_POINT('Origin',(1.9,3.,3.1));
#6340=CARTESIAN_POINT('Origin',(-1.9,-3.1,6.9));
#6341=CARTESIAN_POINT('',(-2.175,0.0249999999999999,6.9));
#6342=CARTESIAN_POINT('Origin',(-1.9,0.0249999999999999,6.9));
#6343=CARTESIAN_POINT('',(-2.175,3.,6.9));
#6344=CARTESIAN_POINT('',(-2.175,-3.1,6.9));
#6345=CARTESIAN_POINT('Origin',(-1.9,3.,6.9));
#6346=CARTESIAN_POINT('Origin',(-1.9,-3.1,3.1));
#6347=CARTESIAN_POINT('',(-2.175,0.0249999999999999,3.1));
#6348=CARTESIAN_POINT('Origin',(-1.9,0.0249999999999999,3.1));
#6349=CARTESIAN_POINT('',(-2.175,3.,3.1));
#6350=CARTESIAN_POINT('',(-2.175,-3.1,3.1));
#6351=CARTESIAN_POINT('Origin',(-1.9,3.,3.1));
#6352=CARTESIAN_POINT('Origin',(1.9,-3.1,6.9));
#6353=CARTESIAN_POINT('',(1.625,0.0249999999999999,6.9));
#6354=CARTESIAN_POINT('Origin',(1.9,0.0249999999999999,6.9));
#6355=CARTESIAN_POINT('',(1.625,3.,6.9));
#6356=CARTESIAN_POINT('',(1.625,-3.1,6.9));
#6357=CARTESIAN_POINT('Origin',(1.9,3.,6.9));
#6358=CARTESIAN_POINT('Origin',(0.,0.,6.5));
#6359=CARTESIAN_POINT('',(-0.699553428981661,0.025,6.5));
#6360=CARTESIAN_POINT('',(-0.699553428981661,0.025,7.5));
#6361=CARTESIAN_POINT('',(-0.699553428981661,0.025,6.5));
#6362=CARTESIAN_POINT('',(0.699553428981661,0.025,6.5));
#6363=CARTESIAN_POINT('Origin',(0.,0.,6.5));
#6364=CARTESIAN_POINT('',(0.699553428981661,0.025,7.5));
#6365=CARTESIAN_POINT('',(0.699553428981661,0.025,6.5));
#6366=CARTESIAN_POINT('Origin',(0.,0.,7.5));
#6367=CARTESIAN_POINT('Origin',(0.,0.,6.5));
#6368=CARTESIAN_POINT('',(-0.556214886532175,0.025,6.5));
#6369=CARTESIAN_POINT('',(-1.25,0.025,6.5));
#6370=CARTESIAN_POINT('',(0.556214886532175,0.025,6.5));
#6371=CARTESIAN_POINT('Origin',(0.,0.,6.5));
#6372=CARTESIAN_POINT('',(-1.25,0.025,6.5));
#6373=CARTESIAN_POINT('Origin',(0.,1.5125,7.5));
#6374=CARTESIAN_POINT('',(2.5,0.0249999999999999,7.5));
#6375=CARTESIAN_POINT('',(-2.5,0.025,7.5));
#6376=CARTESIAN_POINT('',(2.5,3.,7.5));
#6377=CARTESIAN_POINT('',(2.5,0.025,7.5));
#6378=CARTESIAN_POINT('',(-2.5,3.,7.5));
#6379=CARTESIAN_POINT('',(2.5,3.,7.5));
#6380=CARTESIAN_POINT('',(-2.5,0.0249999999999999,7.5));
#6381=CARTESIAN_POINT('',(-2.5,3.,7.5));
#6382=CARTESIAN_POINT('',(-2.5,0.025,7.5));
#6383=CARTESIAN_POINT('Origin',(0.,1.8,5.));
#6384=CARTESIAN_POINT('',(-0.93,1.8,5.));
#6385=CARTESIAN_POINT('Origin',(0.,1.8,5.));
#6386=CARTESIAN_POINT('',(-0.93,3.,5.));
#6387=CARTESIAN_POINT('',(-0.93,1.8,5.));
#6388=CARTESIAN_POINT('Origin',(0.,3.,5.));
#6389=CARTESIAN_POINT('Origin',(0.,1.,5.));
#6390=CARTESIAN_POINT('',(-1.3,1.,5.));
#6391=CARTESIAN_POINT('Origin',(0.,1.,5.));
#6392=CARTESIAN_POINT('',(-1.3,1.8,5.));
#6393=CARTESIAN_POINT('',(-1.3,1.,5.));
#6394=CARTESIAN_POINT('Origin',(0.,1.8,5.));
#6395=CARTESIAN_POINT('Origin',(0.,1.8,5.));
#6396=CARTESIAN_POINT('Origin',(0.,1.,5.));
#6397=CARTESIAN_POINT('',(-1.52958336188405E-16,1.,3.75100040032032));
#6398=CARTESIAN_POINT('Origin',(0.,1.,5.));
#6399=CARTESIAN_POINT('Origin',(0.,0.,5.));
#6400=CARTESIAN_POINT('Origin',(0.,0.025,5.));
#6401=CARTESIAN_POINT('Origin',(2.5,3.,2.5));
#6402=CARTESIAN_POINT('',(2.5,3.,2.5));
#6403=CARTESIAN_POINT('',(-2.5,3.,2.5));
#6404=CARTESIAN_POINT('',(2.5,3.,2.5));
#6405=CARTESIAN_POINT('',(-2.5,3.,2.5));
#6406=CARTESIAN_POINT('',(2.5,3.,2.5));
#6407=CARTESIAN_POINT('Origin',(2.5,0.025,2.5));
#6408=CARTESIAN_POINT('',(2.5,0.025,2.5));
#6409=CARTESIAN_POINT('',(2.5,0.025,2.5));
#6410=CARTESIAN_POINT('',(2.5,0.025,2.5));
#6411=CARTESIAN_POINT('Origin',(-2.5,0.025,2.5));
#6412=CARTESIAN_POINT('',(-2.5,0.0249999999999999,2.5));
#6413=CARTESIAN_POINT('',(-2.5,0.0249999999999999,2.5));
#6414=CARTESIAN_POINT('',(-2.5,0.025,2.5));
#6415=CARTESIAN_POINT('Origin',(-2.5,3.,2.5));
#6416=CARTESIAN_POINT('',(-2.5,3.,2.5));
#6417=CARTESIAN_POINT('Origin',(0.,1.5125,2.5));
#6418=CARTESIAN_POINT('',(0.,0.,0.));
#6419=CARTESIAN_POINT('Origin',(0.,0.,5.));
#6420=CARTESIAN_POINT('',(-1.36919674566051E-16,1.,3.88196601125011));
#6421=CARTESIAN_POINT('Origin',(0.,1.,5.));
#6422=CARTESIAN_POINT('',(-0.75,1.29903810567666,5.));
#6423=CARTESIAN_POINT('Origin',(0.,1.29903810567666,5.));
#6424=CARTESIAN_POINT('Origin',(0.,1.,5.));
#6425=CARTESIAN_POINT('',(-0.75,1.8,5.));
#6426=CARTESIAN_POINT('Origin',(0.,1.8,5.));
#6427=CARTESIAN_POINT('',(-0.75,1.,5.));
#6428=CARTESIAN_POINT('Origin',(0.,1.,5.));
#6429=CARTESIAN_POINT('',(-1.3,1.8,5.));
#6430=CARTESIAN_POINT('Origin',(0.,1.8,5.));
#6431=CARTESIAN_POINT('',(-1.3,1.,5.));
#6432=CARTESIAN_POINT('',(-1.3,1.,5.));
#6433=CARTESIAN_POINT('Origin',(0.,1.,5.));
#6434=CARTESIAN_POINT('Origin',(0.,1.8,5.));
#6435=CARTESIAN_POINT('Origin',(0.,1.,5.));
#6436=CARTESIAN_POINT('',(0.,0.,0.));
#6437=CARTESIAN_POINT('Origin',(1.9,-0.1,3.1));
#6438=CARTESIAN_POINT('',(1.625,-0.025,3.1));
#6439=CARTESIAN_POINT('Origin',(1.9,-0.025,3.1));
#6440=CARTESIAN_POINT('',(1.625,0.025,3.1));
#6441=CARTESIAN_POINT('',(1.625,-0.1,3.1));
#6442=CARTESIAN_POINT('Origin',(1.9,0.025,3.1));
#6443=CARTESIAN_POINT('Origin',(-1.9,-0.1,6.9));
#6444=CARTESIAN_POINT('',(-2.175,-0.025,6.9));
#6445=CARTESIAN_POINT('Origin',(-1.9,-0.025,6.9));
#6446=CARTESIAN_POINT('',(-2.175,0.025,6.9));
#6447=CARTESIAN_POINT('',(-2.175,-0.1,6.9));
#6448=CARTESIAN_POINT('Origin',(-1.9,0.025,6.9));
#6449=CARTESIAN_POINT('Origin',(-1.9,-0.1,3.1));
#6450=CARTESIAN_POINT('',(-2.175,-0.025,3.1));
#6451=CARTESIAN_POINT('Origin',(-1.9,-0.025,3.1));
#6452=CARTESIAN_POINT('',(-2.175,0.025,3.1));
#6453=CARTESIAN_POINT('',(-2.175,-0.1,3.1));
#6454=CARTESIAN_POINT('Origin',(-1.9,0.025,3.1));
#6455=CARTESIAN_POINT('Origin',(1.9,-0.1,6.9));
#6456=CARTESIAN_POINT('',(1.625,-0.025,6.9));
#6457=CARTESIAN_POINT('Origin',(1.9,-0.025,6.9));
#6458=CARTESIAN_POINT('',(1.625,0.025,6.9));
#6459=CARTESIAN_POINT('',(1.625,-0.1,6.9));
#6460=CARTESIAN_POINT('Origin',(1.9,0.025,6.9));
#6461=CARTESIAN_POINT('Origin',(-0.7,-0.1,6.5));
#6462=CARTESIAN_POINT('',(-0.7,-0.025,6.5));
#6463=CARTESIAN_POINT('',(-0.7,-0.025,7.5));
#6464=CARTESIAN_POINT('',(-0.7,-0.025,5.75));
#6465=CARTESIAN_POINT('',(-0.7,0.025,6.5));
#6466=CARTESIAN_POINT('',(-0.7,-0.1,6.5));
#6467=CARTESIAN_POINT('',(-0.7,0.025,7.5));
#6468=CARTESIAN_POINT('',(-0.7,0.025,5.75));
#6469=CARTESIAN_POINT('',(-0.7,-0.0625,7.5));
#6470=CARTESIAN_POINT('Origin',(0.7,-0.1,6.5));
#6471=CARTESIAN_POINT('',(0.7,-0.025,6.5));
#6472=CARTESIAN_POINT('',(0.556776436283003,-0.025,6.5));
#6473=CARTESIAN_POINT('',(0.35,-0.025,6.5));
#6474=CARTESIAN_POINT('',(0.7,0.025,6.5));
#6475=CARTESIAN_POINT('',(0.7,-0.1,6.5));
#6476=CARTESIAN_POINT('',(0.556776436283003,0.025,6.5));
#6477=CARTESIAN_POINT('',(0.35,0.025,6.5));
#6478=CARTESIAN_POINT('',(0.556776436283003,-0.1,6.5));
#6479=CARTESIAN_POINT('Origin',(0.7,-0.1,6.5));
#6480=CARTESIAN_POINT('',(-0.556776436283003,-0.025,6.5));
#6481=CARTESIAN_POINT('',(0.35,-0.025,6.5));
#6482=CARTESIAN_POINT('',(-0.556776436283003,0.025,6.5));
#6483=CARTESIAN_POINT('',(-0.556776436283003,-0.1,6.5));
#6484=CARTESIAN_POINT('',(0.35,0.025,6.5));
#6485=CARTESIAN_POINT('Origin',(0.7,-0.1,7.6));
#6486=CARTESIAN_POINT('',(0.7,-0.025,7.5));
#6487=CARTESIAN_POINT('',(0.7,-0.025,6.3));
#6488=CARTESIAN_POINT('',(0.7,0.025,7.5));
#6489=CARTESIAN_POINT('',(0.7,-0.0625,7.5));
#6490=CARTESIAN_POINT('',(0.7,0.025,6.3));
#6491=CARTESIAN_POINT('Origin',(0.,0.025,5.));
#6492=CARTESIAN_POINT('Origin',(0.,0.025,5.));
#6493=CARTESIAN_POINT('',(2.5,0.025,7.5));
#6494=CARTESIAN_POINT('',(2.5,0.025,7.5));
#6495=CARTESIAN_POINT('',(2.5,0.025,2.5));
#6496=CARTESIAN_POINT('',(2.5,0.025,2.5));
#6497=CARTESIAN_POINT('',(-2.5,0.025,2.5));
#6498=CARTESIAN_POINT('',(-2.5,0.025,2.5));
#6499=CARTESIAN_POINT('',(-2.5,0.025,7.5));
#6500=CARTESIAN_POINT('',(-2.5,0.025,7.5));
#6501=CARTESIAN_POINT('',(2.5,0.025,7.5));
#6502=CARTESIAN_POINT('Origin',(-2.5,-0.025,7.5));
#6503=CARTESIAN_POINT('',(2.5,-0.025,7.5));
#6504=CARTESIAN_POINT('',(2.5,-0.025,7.5));
#6505=CARTESIAN_POINT('',(2.5,-0.025,7.5));
#6506=CARTESIAN_POINT('Origin',(-2.5,-0.025,7.5));
#6507=CARTESIAN_POINT('',(-2.5,-0.025,7.5));
#6508=CARTESIAN_POINT('',(-2.5,-0.025,7.5));
#6509=CARTESIAN_POINT('',(2.5,-0.025,7.5));
#6510=CARTESIAN_POINT('Origin',(0.,-0.1,5.));
#6511=CARTESIAN_POINT('Origin',(0.,-0.025,5.));
#6512=CARTESIAN_POINT('Origin',(-2.5,-0.025,2.5));
#6513=CARTESIAN_POINT('',(-2.5,-0.025,2.5));
#6514=CARTESIAN_POINT('',(-2.5,-0.025,7.5));
#6515=CARTESIAN_POINT('',(-2.5,-0.025,2.5));
#6516=CARTESIAN_POINT('Origin',(2.5,-0.025,2.5));
#6517=CARTESIAN_POINT('',(2.5,-0.025,2.5));
#6518=CARTESIAN_POINT('',(-2.5,-0.025,2.5));
#6519=CARTESIAN_POINT('',(2.5,-0.025,2.5));
#6520=CARTESIAN_POINT('Origin',(2.5,-0.025,7.5));
#6521=CARTESIAN_POINT('',(2.5,-0.025,2.5));
#6522=CARTESIAN_POINT('Origin',(0.,-0.025,5.));
#6523=CARTESIAN_POINT('',(0.,0.,0.));
#6524=CARTESIAN_POINT('Origin',(0.,0.,7.5));
#6525=CARTESIAN_POINT('',(-1.2,-1.46957615897682E-16,7.5));
#6526=CARTESIAN_POINT('Origin',(0.,0.,7.5));
#6527=CARTESIAN_POINT('',(-0.7,-8.57252759403147E-17,7.5));
#6528=CARTESIAN_POINT('Origin',(0.,0.,7.5));
#6529=CARTESIAN_POINT('Origin',(0.,0.,7.5));
#6530=CARTESIAN_POINT('',(-1.2,-1.46957615897682E-16,8.));
#6531=CARTESIAN_POINT('Origin',(0.,0.,8.));
#6532=CARTESIAN_POINT('',(-1.2,-1.46957615897682E-16,7.5));
#6533=CARTESIAN_POINT('Origin',(0.,0.,8.));
#6534=CARTESIAN_POINT('',(-0.405,-4.95981953654678E-17,8.));
#6535=CARTESIAN_POINT('Origin',(0.,0.,8.));
#6536=CARTESIAN_POINT('Origin',(0.,0.,6.6));
#6537=CARTESIAN_POINT('',(-0.405,-4.95981953654678E-17,6.6));
#6538=CARTESIAN_POINT('',(-0.405,-4.95981953654678E-17,6.6));
#6539=CARTESIAN_POINT('Origin',(0.,0.,6.6));
#6540=CARTESIAN_POINT('Origin',(0.,0.,6.6));
#6541=CARTESIAN_POINT('',(-0.7,-8.57252759403147E-17,6.6));
#6542=CARTESIAN_POINT('',(-0.7,-8.57252759403147E-17,6.6));
#6543=CARTESIAN_POINT('Origin',(0.,0.,6.6));
#6544=CARTESIAN_POINT('Origin',(0.,0.,6.6));
#6545=CARTESIAN_POINT('',(0.,0.,0.));
#6546=CARTESIAN_POINT('Origin',(0.,0.,8.1));
#6547=CARTESIAN_POINT('',(-0.4,-4.89858719658941E-17,8.1));
#6548=CARTESIAN_POINT('Origin',(-0.5,-6.12323399573677E-17,8.1));
#6549=CARTESIAN_POINT('Origin',(0.,0.,8.1));
#6550=CARTESIAN_POINT('',(0.,0.,0.));
#6551=CARTESIAN_POINT('Origin',(0.,0.,7.9));
#6552=CARTESIAN_POINT('',(-0.61,-7.47034547479885E-17,8.));
#6553=CARTESIAN_POINT('Origin',(0.,0.,8.));
#6554=CARTESIAN_POINT('',(-0.61,-7.47034547479885E-17,8.3));
#6555=CARTESIAN_POINT('',(-0.61,-7.47034547479885E-17,7.9));
#6556=CARTESIAN_POINT('Origin',(0.,0.,8.3));
#6557=CARTESIAN_POINT('Origin',(0.,0.,8.3));
#6558=CARTESIAN_POINT('',(-0.405,4.95981953654678E-17,8.3));
#6559=CARTESIAN_POINT('Origin',(0.,0.,8.3));
#6560=CARTESIAN_POINT('Origin',(0.,0.,8.));
#6561=CARTESIAN_POINT('',(-0.405,-4.95981953654678E-17,8.7));
#6562=CARTESIAN_POINT('Origin',(0.,0.,8.7));
#6563=CARTESIAN_POINT('',(-0.405,-4.95981953654678E-17,8.));
#6564=CARTESIAN_POINT('Origin',(0.,0.,8.));
#6565=CARTESIAN_POINT('',(-1.,-1.22464679914735E-16,8.7));
#6566=CARTESIAN_POINT('Origin',(0.,0.,8.7));
#6567=CARTESIAN_POINT('',(-1.,-1.22464679914735E-16,8.));
#6568=CARTESIAN_POINT('',(-1.,-1.22464679914735E-16,8.));
#6569=CARTESIAN_POINT('Origin',(0.,0.,8.));
#6570=CARTESIAN_POINT('Origin',(0.,0.,8.7));
#6571=CARTESIAN_POINT('Origin',(0.,0.,8.));
#6572=CARTESIAN_POINT('',(0.,0.,0.));
#6573=CARTESIAN_POINT('Origin',(-1.1,-3.,8.1));
#6574=CARTESIAN_POINT('',(-1.4,-3.,8.1));
#6575=CARTESIAN_POINT('Origin',(-1.1,-3.,8.1));
#6576=CARTESIAN_POINT('',(-1.4,-3.,8.5));
#6577=CARTESIAN_POINT('',(-1.4,-3.,8.1));
#6578=CARTESIAN_POINT('Origin',(-1.1,-3.,8.5));
#6579=CARTESIAN_POINT('Origin',(-1.1,-3.,8.1));
#6580=CARTESIAN_POINT('Origin',(3.,1.1,8.1));
#6581=CARTESIAN_POINT('',(2.7,1.1,8.1));
#6582=CARTESIAN_POINT('Origin',(3.,1.1,8.1));
#6583=CARTESIAN_POINT('',(2.7,1.1,8.5));
#6584=CARTESIAN_POINT('',(2.7,1.1,8.1));
#6585=CARTESIAN_POINT('Origin',(3.,1.1,8.5));
#6586=CARTESIAN_POINT('Origin',(3.,1.1,8.1));
#6587=CARTESIAN_POINT('Origin',(1.3,-1.,7.9));
#6588=CARTESIAN_POINT('',(1.075,-1.,8.));
#6589=CARTESIAN_POINT('Origin',(1.3,-1.,8.));
#6590=CARTESIAN_POINT('',(1.075,-1.,8.5));
#6591=CARTESIAN_POINT('',(1.075,-1.,7.9));
#6592=CARTESIAN_POINT('Origin',(1.3,-1.,8.5));
#6593=CARTESIAN_POINT('Origin',(-1.3,1.,7.9));
#6594=CARTESIAN_POINT('',(-1.525,1.,8.));
#6595=CARTESIAN_POINT('Origin',(-1.3,1.,8.));
#6596=CARTESIAN_POINT('',(-1.525,1.,8.5));
#6597=CARTESIAN_POINT('',(-1.525,1.,7.9));
#6598=CARTESIAN_POINT('Origin',(-1.3,1.,8.5));
#6599=CARTESIAN_POINT('Origin',(-1.3,-1.,7.9));
#6600=CARTESIAN_POINT('',(-1.525,-1.,8.));
#6601=CARTESIAN_POINT('Origin',(-1.3,-1.,8.));
#6602=CARTESIAN_POINT('',(-1.525,-1.,8.5));
#6603=CARTESIAN_POINT('',(-1.525,-1.,7.9));
#6604=CARTESIAN_POINT('Origin',(-1.3,-1.,8.5));
#6605=CARTESIAN_POINT('Origin',(1.3,1.,7.9));
#6606=CARTESIAN_POINT('',(1.075,1.,8.));
#6607=CARTESIAN_POINT('Origin',(1.3,1.,8.));
#6608=CARTESIAN_POINT('',(1.075,1.,8.5));
#6609=CARTESIAN_POINT('',(1.075,1.,7.9));
#6610=CARTESIAN_POINT('Origin',(1.3,1.,8.5));
#6611=CARTESIAN_POINT('Origin',(0.,0.,7.9));
#6612=CARTESIAN_POINT('',(-1.01,-1.23689326713883E-16,8.));
#6613=CARTESIAN_POINT('Origin',(0.,0.,8.));
#6614=CARTESIAN_POINT('',(-1.01,1.23689326713883E-16,8.5));
#6615=CARTESIAN_POINT('',(-1.01,-1.23689326713883E-16,7.9));
#6616=CARTESIAN_POINT('Origin',(0.,0.,8.5));
#6617=CARTESIAN_POINT('Origin',(4.,1.5,8.));
#6618=CARTESIAN_POINT('',(4.,1.5,8.));
#6619=CARTESIAN_POINT('',(-2.5,1.5,8.));
#6620=CARTESIAN_POINT('',(4.,1.5,8.));
#6621=CARTESIAN_POINT('',(-2.5,1.5,8.5));
#6622=CARTESIAN_POINT('',(-2.5,1.5,8.));
#6623=CARTESIAN_POINT('',(4.,1.5,8.5));
#6624=CARTESIAN_POINT('',(4.,1.5,8.5));
#6625=CARTESIAN_POINT('',(4.,1.5,8.));
#6626=CARTESIAN_POINT('Origin',(4.,-4.,8.));
#6627=CARTESIAN_POINT('',(4.,-4.,8.));
#6628=CARTESIAN_POINT('',(4.,-4.,8.));
#6629=CARTESIAN_POINT('',(4.,-4.,8.5));
#6630=CARTESIAN_POINT('',(4.,-4.,8.5));
#6631=CARTESIAN_POINT('',(4.,-4.,8.));
#6632=CARTESIAN_POINT('Origin',(-2.5,-4.,8.));
#6633=CARTESIAN_POINT('',(-2.5,-4.,8.));
#6634=CARTESIAN_POINT('',(-2.5,-4.,8.));
#6635=CARTESIAN_POINT('',(-2.5,-4.,8.5));
#6636=CARTESIAN_POINT('',(-2.5,-4.,8.5));
#6637=CARTESIAN_POINT('',(-2.5,-4.,8.));
#6638=CARTESIAN_POINT('Origin',(-2.5,1.5,8.));
#6639=CARTESIAN_POINT('',(-2.5,1.5,8.));
#6640=CARTESIAN_POINT('',(-2.5,1.5,8.5));
#6641=CARTESIAN_POINT('Origin',(0.75,-1.25,8.5));
#6642=CARTESIAN_POINT('Origin',(0.75,-1.25,8.));
#6643=CARTESIAN_POINT('',(0.,0.,0.));
#6644=CARTESIAN_POINT('Origin',(-1.3,-1.,7.5));
#6645=CARTESIAN_POINT('',(-1.525,-1.,8.));
#6646=CARTESIAN_POINT('Origin',(-1.3,-1.,8.));
#6647=CARTESIAN_POINT('',(-1.525,-1.,7.5));
#6648=CARTESIAN_POINT('',(-1.525,-1.,7.5));
#6649=CARTESIAN_POINT('Origin',(-1.3,-1.,7.5));
#6650=CARTESIAN_POINT('Origin',(-1.3,-1.,7.5));
#6651=CARTESIAN_POINT('',(-1.7,-1.,8.));
#6652=CARTESIAN_POINT('Origin',(-1.3,-1.,8.));
#6653=CARTESIAN_POINT('',(-1.7,-1.,7.5));
#6654=CARTESIAN_POINT('',(-1.7,-1.,7.5));
#6655=CARTESIAN_POINT('Origin',(-1.3,-1.,7.5));
#6656=CARTESIAN_POINT('Origin',(-1.3,-1.,8.));
#6657=CARTESIAN_POINT('Origin',(-1.3,-1.,7.5));
#6658=CARTESIAN_POINT('',(0.,0.,0.));
#6659=CARTESIAN_POINT('Origin',(-1.3,1.,7.5));
#6660=CARTESIAN_POINT('',(-1.525,1.,8.));
#6661=CARTESIAN_POINT('Origin',(-1.3,1.,8.));
#6662=CARTESIAN_POINT('',(-1.525,1.,7.5));
#6663=CARTESIAN_POINT('',(-1.525,1.,7.5));
#6664=CARTESIAN_POINT('Origin',(-1.3,1.,7.5));
#6665=CARTESIAN_POINT('Origin',(-1.3,1.,7.5));
#6666=CARTESIAN_POINT('',(-1.7,1.,8.));
#6667=CARTESIAN_POINT('Origin',(-1.3,1.,8.));
#6668=CARTESIAN_POINT('',(-1.7,1.,7.5));
#6669=CARTESIAN_POINT('',(-1.7,1.,7.5));
#6670=CARTESIAN_POINT('Origin',(-1.3,1.,7.5));
#6671=CARTESIAN_POINT('Origin',(-1.3,1.,8.));
#6672=CARTESIAN_POINT('Origin',(-1.3,1.,7.5));
#6673=CARTESIAN_POINT('',(0.,0.,0.));
#6674=CARTESIAN_POINT('Origin',(1.3,-1.,7.5));
#6675=CARTESIAN_POINT('',(1.075,-1.,8.));
#6676=CARTESIAN_POINT('Origin',(1.3,-1.,8.));
#6677=CARTESIAN_POINT('',(1.075,-1.,7.5));
#6678=CARTESIAN_POINT('',(1.075,-1.,7.5));
#6679=CARTESIAN_POINT('Origin',(1.3,-1.,7.5));
#6680=CARTESIAN_POINT('Origin',(1.3,-1.,7.5));
#6681=CARTESIAN_POINT('',(0.9,-1.,8.));
#6682=CARTESIAN_POINT('Origin',(1.3,-1.,8.));
#6683=CARTESIAN_POINT('',(0.9,-1.,7.5));
#6684=CARTESIAN_POINT('',(0.9,-1.,7.5));
#6685=CARTESIAN_POINT('Origin',(1.3,-1.,7.5));
#6686=CARTESIAN_POINT('Origin',(1.3,-1.,8.));
#6687=CARTESIAN_POINT('Origin',(1.3,-1.,7.5));
#6688=CARTESIAN_POINT('',(0.,0.,0.));
#6689=CARTESIAN_POINT('Origin',(1.3,1.,7.5));
#6690=CARTESIAN_POINT('',(1.075,1.,8.));
#6691=CARTESIAN_POINT('Origin',(1.3,1.,8.));
#6692=CARTESIAN_POINT('',(1.075,1.,7.5));
#6693=CARTESIAN_POINT('',(1.075,1.,7.5));
#6694=CARTESIAN_POINT('Origin',(1.3,1.,7.5));
#6695=CARTESIAN_POINT('Origin',(1.3,1.,7.5));
#6696=CARTESIAN_POINT('',(0.9,1.,8.));
#6697=CARTESIAN_POINT('Origin',(1.3,1.,8.));
#6698=CARTESIAN_POINT('',(0.9,1.,7.5));
#6699=CARTESIAN_POINT('',(0.9,1.,7.5));
#6700=CARTESIAN_POINT('Origin',(1.3,1.,7.5));
#6701=CARTESIAN_POINT('Origin',(1.3,1.,8.));
#6702=CARTESIAN_POINT('Origin',(1.3,1.,7.5));
#6703=CARTESIAN_POINT('',(0.,0.,0.));
#6704=CARTESIAN_POINT('Origin',(3.,1.1,8.2));
#6705=CARTESIAN_POINT('',(2.7,1.1,9.4));
#6706=CARTESIAN_POINT('Origin',(3.,1.1,9.4));
#6707=CARTESIAN_POINT('',(2.7,1.1,8.2));
#6708=CARTESIAN_POINT('',(2.7,1.1,8.2));
#6709=CARTESIAN_POINT('Origin',(3.,1.1,8.2));
#6710=CARTESIAN_POINT('Origin',(3.,1.1,9.4));
#6711=CARTESIAN_POINT('Origin',(3.,1.1,8.2));
#6712=CARTESIAN_POINT('',(0.,0.,0.));
#6713=CARTESIAN_POINT('Origin',(-1.1,-3.,8.2));
#6714=CARTESIAN_POINT('',(-1.4,-3.,9.4));
#6715=CARTESIAN_POINT('Origin',(-1.1,-3.,9.4));
#6716=CARTESIAN_POINT('',(-1.4,-3.,8.2));
#6717=CARTESIAN_POINT('',(-1.4,-3.,8.2));
#6718=CARTESIAN_POINT('Origin',(-1.1,-3.,8.2));
#6719=CARTESIAN_POINT('Origin',(-1.1,-3.,9.4));
#6720=CARTESIAN_POINT('Origin',(-1.1,-3.,8.2));
#6721=CARTESIAN_POINT('',(0.,0.,0.));
#6722=CARTESIAN_POINT('Origin',(0.115470053837925,-0.5,-0.2));
#6723=CARTESIAN_POINT('',(0.23094010767585,-0.5,0.));
#6724=CARTESIAN_POINT('',(0.115470053837925,-0.5,-0.2));
#6725=CARTESIAN_POINT('',(0.23094010767585,-0.5,0.));
#6726=CARTESIAN_POINT('',(0.115470053837925,-0.8,-0.2));
#6727=CARTESIAN_POINT('',(0.115470053837925,-0.5,-0.2));
#6728=CARTESIAN_POINT('',(0.23094010767585,-0.8,0.));
#6729=CARTESIAN_POINT('',(0.23094010767585,-0.8,0.));
#6730=CARTESIAN_POINT('',(0.23094010767585,-0.5,0.));
#6731=CARTESIAN_POINT('Origin',(-0.115470053837925,-0.5,-0.2));
#6732=CARTESIAN_POINT('',(-0.115470053837925,-0.5,-0.2));
#6733=CARTESIAN_POINT('',(0.115470053837925,-0.5,-0.2));
#6734=CARTESIAN_POINT('',(-0.115470053837925,-0.8,-0.2));
#6735=CARTESIAN_POINT('',(-0.115470053837925,-0.5,-0.2));
#6736=CARTESIAN_POINT('',(0.115470053837925,-0.8,-0.2));
#6737=CARTESIAN_POINT('Origin',(-0.23094010767585,-0.5,-2.77555756156289E-17));
#6738=CARTESIAN_POINT('',(-0.23094010767585,-0.5,-2.82820063659975E-17));
#6739=CARTESIAN_POINT('',(-0.115470053837925,-0.5,-0.2));
#6740=CARTESIAN_POINT('',(-0.23094010767585,-0.8,-2.77555756156289E-17));
#6741=CARTESIAN_POINT('',(-0.23094010767585,-0.5,-2.82820063659975E-17));
#6742=CARTESIAN_POINT('',(-0.115470053837925,-0.8,-0.2));
#6743=CARTESIAN_POINT('Origin',(-0.115470053837925,-0.5,0.2));
#6744=CARTESIAN_POINT('',(-0.115470053837925,-0.5,0.2));
#6745=CARTESIAN_POINT('',(-0.23094010767585,-0.5,-2.82820063659975E-17));
#6746=CARTESIAN_POINT('',(-0.115470053837925,-0.8,0.2));
#6747=CARTESIAN_POINT('',(-0.115470053837925,-0.5,0.2));
#6748=CARTESIAN_POINT('',(-0.23094010767585,-0.8,-2.82820063659975E-17));
#6749=CARTESIAN_POINT('Origin',(0.115470053837925,-0.5,0.2));
#6750=CARTESIAN_POINT('',(0.115470053837925,-0.5,0.2));
#6751=CARTESIAN_POINT('',(-0.115470053837925,-0.5,0.2));
#6752=CARTESIAN_POINT('',(0.115470053837925,-0.8,0.2));
#6753=CARTESIAN_POINT('',(0.115470053837925,-0.5,0.2));
#6754=CARTESIAN_POINT('',(-0.115470053837925,-0.8,0.2));
#6755=CARTESIAN_POINT('Origin',(0.23094010767585,-0.5,0.));
#6756=CARTESIAN_POINT('',(0.115470053837925,-0.5,0.2));
#6757=CARTESIAN_POINT('',(0.115470053837925,-0.8,0.2));
#6758=CARTESIAN_POINT('Origin',(0.,-0.5,0.));
#6759=CARTESIAN_POINT('Origin',(0.,-0.8,0.));
#6760=CARTESIAN_POINT('Origin',(0.,-1.9,0.));
#6761=CARTESIAN_POINT('',(-0.25,-1.9,3.06161699786838E-17));
#6762=CARTESIAN_POINT('Origin',(0.,-1.9,0.));
#6763=CARTESIAN_POINT('',(-0.24505,-1.9,3.00099698131059E-17));
#6764=CARTESIAN_POINT('Origin',(0.,-1.9,0.));
#6765=CARTESIAN_POINT('Origin',(0.,-7.,0.));
#6766=CARTESIAN_POINT('',(-0.25,-7.,3.06161699786838E-17));
#6767=CARTESIAN_POINT('',(-0.25,-7.,3.06161699786838E-17));
#6768=CARTESIAN_POINT('Origin',(0.,-7.,0.));
#6769=CARTESIAN_POINT('Origin',(0.,-7.,0.));
#6770=CARTESIAN_POINT('Origin',(0.375,0.5,0.));
#6771=CARTESIAN_POINT('',(-0.375,0.5,-4.59242549680257E-17));
#6772=CARTESIAN_POINT('Origin',(0.,0.5,0.));
#6773=CARTESIAN_POINT('Origin',(0.,0.475,0.));
#6774=CARTESIAN_POINT('',(-0.425,0.45,-5.20474889637625E-17));
#6775=CARTESIAN_POINT('Origin',(0.,0.45,0.));
#6776=CARTESIAN_POINT('',(-0.4,0.475,-4.89858719658941E-17));
#6777=CARTESIAN_POINT('Origin',(0.,0.24,0.));
#6778=CARTESIAN_POINT('',(-0.425,0.0299999999999998,-5.20474889637625E-17));
#6779=CARTESIAN_POINT('Origin',(0.,0.0299999999999998,0.));
#6780=CARTESIAN_POINT('',(-0.425,0.24,-5.20474889637625E-17));
#6781=CARTESIAN_POINT('Origin',(0.,0.0150000000000001,0.));
#6782=CARTESIAN_POINT('',(-0.395,4.85722573273506E-17,-4.83735485663204E-17));
#6783=CARTESIAN_POINT('Origin',(0.,0.,0.));
#6784=CARTESIAN_POINT('',(-0.41,0.0150000000000001,-5.02105187650415E-17));
#6785=CARTESIAN_POINT('Origin',(0.27,0.,0.));
#6786=CARTESIAN_POINT('',(-0.27,0.,-3.30654635769785E-17));
#6787=CARTESIAN_POINT('Origin',(0.,0.,0.));
#6788=CARTESIAN_POINT('Origin',(0.,-0.02,0.));
#6789=CARTESIAN_POINT('',(-0.24505,-0.0498999999999999,3.00099698131059E-17));
#6790=CARTESIAN_POINT('Origin',(0.,-0.0498999999999999,0.));
#6791=CARTESIAN_POINT('',(-0.26,-0.02,-3.18408167778312E-17));
#6792=CARTESIAN_POINT('Origin',(0.,-0.995,0.));
#6793=CARTESIAN_POINT('',(-0.24505,-0.995,-3.00099698131059E-17));
#6794=CARTESIAN_POINT('',(0.,0.,0.));
#6795=CARTESIAN_POINT('Origin',(0.,0.09,0.));
#6796=CARTESIAN_POINT('',(-0.285,0.1,3.49024337756996E-17));
#6797=CARTESIAN_POINT('Origin',(0.,0.1,0.));
#6798=CARTESIAN_POINT('',(-0.265,0.08,-3.24531401774049E-17));
#6799=CARTESIAN_POINT('',(-0.275,0.09,3.36777869765522E-17));
#6800=CARTESIAN_POINT('Origin',(0.,0.08,0.));
#6801=CARTESIAN_POINT('Origin',(0.,0.,0.));
#6802=CARTESIAN_POINT('',(-0.265,0.,3.24531401774049E-17));
#6803=CARTESIAN_POINT('',(-0.265,0.,3.24531401774049E-17));
#6804=CARTESIAN_POINT('Origin',(0.,0.,0.));
#6805=CARTESIAN_POINT('Origin',(0.,0.1,0.));
#6806=CARTESIAN_POINT('',(-0.5,0.1,6.12323399573677E-17));
#6807=CARTESIAN_POINT('Origin',(0.,0.1,0.));
#6808=CARTESIAN_POINT('Origin',(0.,0.,0.));
#6809=CARTESIAN_POINT('',(-0.5,0.,6.12323399573677E-17));
#6810=CARTESIAN_POINT('',(-0.5,0.,6.12323399573677E-17));
#6811=CARTESIAN_POINT('Origin',(0.,0.,0.));
#6812=CARTESIAN_POINT('Origin',(0.,0.,0.));
#6813=CARTESIAN_POINT('',(0.,0.,0.));
#6814=CARTESIAN_POINT('Origin',(0.,0.0525042956467857,0.));
#6815=CARTESIAN_POINT('',(-0.230940107675851,0.0472735643746089,0.4));
#6816=CARTESIAN_POINT('',(0.23094010767585,0.0472735643746089,0.4));
#6817=CARTESIAN_POINT('Ctrl Pts',(-0.230940107675851,0.0472735643746089,
0.4));
#6818=CARTESIAN_POINT('Ctrl Pts',(1.11022302462516E-16,-0.0193931022920578,
0.4));
#6819=CARTESIAN_POINT('Ctrl Pts',(0.23094010767585,0.0472735643746089,0.4));
#6820=CARTESIAN_POINT('',(-0.461880215351701,0.0472735643746089,-5.6564012731995E-17));
#6821=CARTESIAN_POINT('Ctrl Pts',(-0.461880215351701,0.0472735643746089,
-5.6564012731995E-17));
#6822=CARTESIAN_POINT('Ctrl Pts',(-0.346410161513776,-0.0193931022920579,
0.2));
#6823=CARTESIAN_POINT('Ctrl Pts',(-0.230940107675851,0.0472735643746089,
0.4));
#6824=CARTESIAN_POINT('',(-0.38,-2.08166817117217E-17,-4.65365783675994E-17));
#6825=CARTESIAN_POINT('',(-0.47094010767585,0.0525042956467857,-5.7673529545534E-17));
#6826=CARTESIAN_POINT('Origin',(0.,0.,0.));
#6827=CARTESIAN_POINT('',(-0.23094010767585,0.0472735643746089,-0.4));
#6828=CARTESIAN_POINT('Ctrl Pts',(-0.23094010767585,0.0472735643746089,
-0.4));
#6829=CARTESIAN_POINT('Ctrl Pts',(-0.346410161513775,-0.0193931022920578,
-0.2));
#6830=CARTESIAN_POINT('Ctrl Pts',(-0.461880215351701,0.0472735643746089,
-5.6564012731995E-17));
#6831=CARTESIAN_POINT('',(0.23094010767585,0.0472735643746089,-0.4));
#6832=CARTESIAN_POINT('Ctrl Pts',(0.23094010767585,0.0472735643746089,-0.4));
#6833=CARTESIAN_POINT('Ctrl Pts',(0.,-0.0193931022920578,-0.4));
#6834=CARTESIAN_POINT('Ctrl Pts',(-0.23094010767585,0.0472735643746089,
-0.4));
#6835=CARTESIAN_POINT('',(0.461880215351701,0.0472735643746089,0.));
#6836=CARTESIAN_POINT('Ctrl Pts',(0.461880215351701,0.0472735643746089,
0.));
#6837=CARTESIAN_POINT('Ctrl Pts',(0.346410161513776,-0.019393102292058,
-0.2));
#6838=CARTESIAN_POINT('Ctrl Pts',(0.23094010767585,0.0472735643746089,-0.4));
#6839=CARTESIAN_POINT('Ctrl Pts',(0.23094010767585,0.0472735643746089,0.4));
#6840=CARTESIAN_POINT('Ctrl Pts',(0.346410161513776,-0.0193931022920577,
0.2));
#6841=CARTESIAN_POINT('Ctrl Pts',(0.461880215351701,0.0472735643746089,
0.));
#6842=CARTESIAN_POINT('Origin',(0.,0.417495704353214,0.));
#6843=CARTESIAN_POINT('',(-0.38,0.47,-4.65365783675994E-17));
#6844=CARTESIAN_POINT('Origin',(0.,0.47,0.));
#6845=CARTESIAN_POINT('',(-0.461880215351701,0.422726435625391,-5.6564012731995E-17));
#6846=CARTESIAN_POINT('',(-0.47094010767585,0.417495704353214,-5.7673529545534E-17));
#6847=CARTESIAN_POINT('',(-0.230940107675851,0.422726435625391,0.4));
#6848=CARTESIAN_POINT('Ctrl Pts',(-0.230940107675851,0.422726435625391,
0.4));
#6849=CARTESIAN_POINT('Ctrl Pts',(-0.346410161513776,0.489393102292058,
0.2));
#6850=CARTESIAN_POINT('Ctrl Pts',(-0.461880215351701,0.422726435625391,
-5.6564012731995E-17));
#6851=CARTESIAN_POINT('',(0.23094010767585,0.422726435625391,0.4));
#6852=CARTESIAN_POINT('Ctrl Pts',(0.23094010767585,0.422726435625391,0.4));
#6853=CARTESIAN_POINT('Ctrl Pts',(8.32667268468867E-17,0.489393102292058,
0.4));
#6854=CARTESIAN_POINT('Ctrl Pts',(-0.230940107675851,0.422726435625391,
0.4));
#6855=CARTESIAN_POINT('',(0.461880215351701,0.422726435625391,0.));
#6856=CARTESIAN_POINT('Ctrl Pts',(0.461880215351701,0.422726435625391,0.));
#6857=CARTESIAN_POINT('Ctrl Pts',(0.346410161513776,0.489393102292058,0.2));
#6858=CARTESIAN_POINT('Ctrl Pts',(0.23094010767585,0.422726435625391,0.4));
#6859=CARTESIAN_POINT('',(0.23094010767585,0.422726435625391,-0.4));
#6860=CARTESIAN_POINT('Ctrl Pts',(0.23094010767585,0.422726435625391,-0.4));
#6861=CARTESIAN_POINT('Ctrl Pts',(0.346410161513775,0.489393102292058,-0.2));
#6862=CARTESIAN_POINT('Ctrl Pts',(0.461880215351701,0.422726435625391,0.));
#6863=CARTESIAN_POINT('',(-0.23094010767585,0.422726435625391,-0.4));
#6864=CARTESIAN_POINT('Ctrl Pts',(-0.23094010767585,0.422726435625391,-0.4));
#6865=CARTESIAN_POINT('Ctrl Pts',(-5.55111512312578E-17,0.489393102292058,
-0.4));
#6866=CARTESIAN_POINT('Ctrl Pts',(0.23094010767585,0.422726435625391,-0.4));
#6867=CARTESIAN_POINT('Ctrl Pts',(-0.461880215351701,0.422726435625391,
-5.6564012731995E-17));
#6868=CARTESIAN_POINT('Ctrl Pts',(-0.346410161513776,0.489393102292058,
-0.2));
#6869=CARTESIAN_POINT('Ctrl Pts',(-0.23094010767585,0.422726435625391,-0.4));
#6870=CARTESIAN_POINT('Origin',(0.23094010767585,0.,-0.4));
#6871=CARTESIAN_POINT('',(-0.23094010767585,0.,-0.4));
#6872=CARTESIAN_POINT('',(0.23094010767585,0.,-0.4));
#6873=CARTESIAN_POINT('Origin',(-0.23094010767585,0.,-0.4));
#6874=CARTESIAN_POINT('',(-0.461880215351701,0.,-5.6564012731995E-17));
#6875=CARTESIAN_POINT('Origin',(-0.461880215351701,0.,-5.6564012731995E-17));
#6876=CARTESIAN_POINT('',(-0.230940107675851,0.,0.4));
#6877=CARTESIAN_POINT('Origin',(0.,0.,0.));
#6878=CARTESIAN_POINT('',(-0.2117,0.47,2.59257727379495E-17));
#6879=CARTESIAN_POINT('Origin',(0.,0.47,0.));
#6880=CARTESIAN_POINT('',(-0.2117,0.,2.59257727379495E-17));
#6881=CARTESIAN_POINT('',(-0.2117,0.,2.59257727379495E-17));
#6882=CARTESIAN_POINT('Origin',(0.,0.,0.));
#6883=CARTESIAN_POINT('Origin',(-0.230940107675851,0.,0.4));
#6884=CARTESIAN_POINT('',(0.23094010767585,0.,0.4));
#6885=CARTESIAN_POINT('Origin',(0.461880215351701,0.,0.));
#6886=CARTESIAN_POINT('',(0.461880215351701,0.,0.));
#6887=CARTESIAN_POINT('Origin',(0.23094010767585,0.,0.4));
#6888=CARTESIAN_POINT('Origin',(0.,0.47,0.));
#6889=CARTESIAN_POINT('Origin',(0.,0.,0.));
#6890=CARTESIAN_POINT('',(0.,0.,0.));
#6891=CARTESIAN_POINT('Origin',(0.,-0.6,0.));
#6892=CARTESIAN_POINT('',(1.55884572681199,-0.6,0.));
#6893=CARTESIAN_POINT('',(0.779422863405995,-0.6,1.35));
#6894=CARTESIAN_POINT('',(0.779422863405995,-0.6,1.35));
#6895=CARTESIAN_POINT('',(-0.779422863405996,-0.6,1.35));
#6896=CARTESIAN_POINT('',(-0.779422863405996,-0.6,1.35));
#6897=CARTESIAN_POINT('',(-1.55884572681199,-0.6,-1.90903542970483E-16));
#6898=CARTESIAN_POINT('',(-1.55884572681199,-0.6,-1.90903542970483E-16));
#6899=CARTESIAN_POINT('',(-0.779422863405995,-0.6,-1.35));
#6900=CARTESIAN_POINT('',(-0.779422863405995,-0.6,-1.35));
#6901=CARTESIAN_POINT('',(0.779422863405995,-0.6,-1.35));
#6902=CARTESIAN_POINT('',(0.779422863405995,-0.6,-1.35));
#6903=CARTESIAN_POINT('',(1.55884572681199,-0.6,0.));
#6904=CARTESIAN_POINT('',(-1.065,-0.6,-1.30424884109193E-16));
#6905=CARTESIAN_POINT('Origin',(0.,-0.6,0.));
#6906=CARTESIAN_POINT('Origin',(0.,0.6,0.));
#6907=CARTESIAN_POINT('',(0.779422863405995,0.6,1.35));
#6908=CARTESIAN_POINT('',(1.55884572681199,0.6,0.));
#6909=CARTESIAN_POINT('',(0.779422863405995,0.6,1.35));
#6910=CARTESIAN_POINT('',(0.779422863405995,0.6,-1.35));
#6911=CARTESIAN_POINT('',(1.55884572681199,0.6,0.));
#6912=CARTESIAN_POINT('',(-0.779422863405995,0.6,-1.35));
#6913=CARTESIAN_POINT('',(0.779422863405995,0.6,-1.35));
#6914=CARTESIAN_POINT('',(-1.55884572681199,0.6,-1.90903542970483E-16));
#6915=CARTESIAN_POINT('',(-0.779422863405995,0.6,-1.35));
#6916=CARTESIAN_POINT('',(-0.779422863405996,0.6,1.35));
#6917=CARTESIAN_POINT('',(-1.55884572681199,0.6,-1.90903542970483E-16));
#6918=CARTESIAN_POINT('',(-0.779422863405996,0.6,1.35));
#6919=CARTESIAN_POINT('',(-1.065,0.6,1.30424884109193E-16));
#6920=CARTESIAN_POINT('Origin',(0.,0.6,0.));
#6921=CARTESIAN_POINT('Origin',(-0.779422863405996,0.,1.35));
#6922=CARTESIAN_POINT('',(0.779422863405995,0.,1.35));
#6923=CARTESIAN_POINT('',(-0.779422863405996,0.,1.35));
#6924=CARTESIAN_POINT('Origin',(-1.55884572681199,0.,-1.90903542970483E-16));
#6925=CARTESIAN_POINT('',(-1.55884572681199,0.,-1.90903542970483E-16));
#6926=CARTESIAN_POINT('Origin',(-0.779422863405995,0.,-1.35));
#6927=CARTESIAN_POINT('',(-0.779422863405995,0.,-1.35));
#6928=CARTESIAN_POINT('Origin',(0.779422863405995,0.,-1.35));
#6929=CARTESIAN_POINT('',(0.779422863405995,0.,-1.35));
#6930=CARTESIAN_POINT('Origin',(1.55884572681199,0.,0.));
#6931=CARTESIAN_POINT('',(1.55884572681199,0.,0.));
#6932=CARTESIAN_POINT('Origin',(0.779422863405995,0.,1.35));
#6933=CARTESIAN_POINT('Origin',(0.,0.,0.));
#6934=CARTESIAN_POINT('',(-1.065,2.47,-1.30424884109193E-16));
#6935=CARTESIAN_POINT('',(-1.065,0.,-1.30424884109193E-16));
#6936=CARTESIAN_POINT('Origin',(0.,2.47,0.));
#6937=CARTESIAN_POINT('Origin',(0.985,2.55,0.));
#6938=CARTESIAN_POINT('',(-0.985,2.55,-1.20627709716014E-16));
#6939=CARTESIAN_POINT('Origin',(0.,2.55,0.));
#6940=CARTESIAN_POINT('',(-0.79,2.55,-9.67470971326409E-17));
#6941=CARTESIAN_POINT('Origin',(0.,2.55,0.));
#6942=CARTESIAN_POINT('Origin',(0.,2.51,0.));
#6943=CARTESIAN_POINT('',(-1.025,2.51,-1.25526296912604E-16));
#6944=CARTESIAN_POINT('Origin',(0.,0.,0.));
#6945=CARTESIAN_POINT('',(-1.065,-2.47,-1.30424884109193E-16));
#6946=CARTESIAN_POINT('Origin',(0.,-2.47,0.));
#6947=CARTESIAN_POINT('',(-1.065,0.,-1.30424884109193E-16));
#6948=CARTESIAN_POINT('Origin',(0.,-2.51,0.));
#6949=CARTESIAN_POINT('',(-0.985,-2.55,-1.20627709716014E-16));
#6950=CARTESIAN_POINT('Origin',(0.,-2.55,0.));
#6951=CARTESIAN_POINT('',(-1.025,-2.51,-1.25526296912604E-16));
#6952=CARTESIAN_POINT('Origin',(0.79,-2.55,0.));
#6953=CARTESIAN_POINT('',(-0.79,-2.55,-9.67470971326409E-17));
#6954=CARTESIAN_POINT('Origin',(0.,-2.55,0.));
#6955=CARTESIAN_POINT('Origin',(0.,0.,0.));
#6956=CARTESIAN_POINT('',(-0.79,0.,-9.67470971326409E-17));
#6957=CARTESIAN_POINT('',(0.,0.,0.));
#6958=CARTESIAN_POINT('Origin',(0.3,0.4,0.));
#6959=CARTESIAN_POINT('',(-0.3,0.4,-3.67394039744206E-17));
#6960=CARTESIAN_POINT('Origin',(0.,0.4,0.));
#6961=CARTESIAN_POINT('Origin',(0.,0.375,0.));
#6962=CARTESIAN_POINT('',(-0.35,0.35,-4.28626379701573E-17));
#6963=CARTESIAN_POINT('Origin',(0.,0.35,0.));
#6964=CARTESIAN_POINT('',(-0.325,0.375,-3.9801020972289E-17));
#6965=CARTESIAN_POINT('Origin',(0.,0.19,0.));
#6966=CARTESIAN_POINT('',(-0.35,0.03,-4.28626379701574E-17));
#6967=CARTESIAN_POINT('Origin',(0.,0.03,0.));
#6968=CARTESIAN_POINT('',(-0.35,0.19,-4.28626379701574E-17));
#6969=CARTESIAN_POINT('Origin',(0.,0.0149999999999999,0.));
#6970=CARTESIAN_POINT('',(-0.32,-3.29597460435593E-17,-3.91886975727153E-17));
#6971=CARTESIAN_POINT('Origin',(0.,0.,0.));
#6972=CARTESIAN_POINT('',(-0.335,0.0149999999999999,-4.10256677714363E-17));
#6973=CARTESIAN_POINT('Origin',(0.22,0.,0.));
#6974=CARTESIAN_POINT('',(-0.22,-6.93889390390723E-18,-2.69422295812418E-17));
#6975=CARTESIAN_POINT('Origin',(0.,0.,0.));
#6976=CARTESIAN_POINT('Origin',(0.,-0.02,0.));
#6977=CARTESIAN_POINT('',(-0.1954,-0.0492,2.39295984553393E-17));
#6978=CARTESIAN_POINT('Origin',(0.,-0.0492,0.));
#6979=CARTESIAN_POINT('',(-0.21,-0.02,-2.57175827820944E-17));
#6980=CARTESIAN_POINT('Origin',(0.,-0.8,0.));
#6981=CARTESIAN_POINT('',(-0.1954,-1.5646,2.39295984553393E-17));
#6982=CARTESIAN_POINT('Origin',(0.,-1.5646,0.));
#6983=CARTESIAN_POINT('',(-0.1954,-0.8,-2.39295984553393E-17));
#6984=CARTESIAN_POINT('Origin',(0.,-1.58,0.));
#6985=CARTESIAN_POINT('',(-0.16,-1.6,-1.95943487863577E-17));
#6986=CARTESIAN_POINT('Origin',(0.,-1.6,0.));
#6987=CARTESIAN_POINT('',(-0.18,-1.58,-2.20436423846524E-17));
#6988=CARTESIAN_POINT('Origin',(0.,-1.6,0.));
#6989=CARTESIAN_POINT('Origin',(0.0866025403784439,-0.4,-0.15));
#6990=CARTESIAN_POINT('',(0.173205080756888,-0.4,0.));
#6991=CARTESIAN_POINT('',(0.0866025403784439,-0.4,-0.15));
#6992=CARTESIAN_POINT('',(0.173205080756888,-0.4,0.));
#6993=CARTESIAN_POINT('',(0.0866025403784439,-0.64,-0.15));
#6994=CARTESIAN_POINT('',(0.0866025403784439,-0.4,-0.15));
#6995=CARTESIAN_POINT('',(0.173205080756888,-0.64,0.));
#6996=CARTESIAN_POINT('',(0.173205080756888,-0.64,0.));
#6997=CARTESIAN_POINT('',(0.173205080756888,-0.4,0.));
#6998=CARTESIAN_POINT('Origin',(-0.0866025403784438,-0.4,-0.15));
#6999=CARTESIAN_POINT('',(-0.0866025403784438,-0.4,-0.15));
#7000=CARTESIAN_POINT('',(0.0866025403784439,-0.4,-0.15));
#7001=CARTESIAN_POINT('',(-0.0866025403784438,-0.64,-0.15));
#7002=CARTESIAN_POINT('',(-0.0866025403784438,-0.4,-0.15));
#7003=CARTESIAN_POINT('',(0.0866025403784439,-0.64,-0.15));
#7004=CARTESIAN_POINT('Origin',(-0.173205080756888,-0.4,-2.77555756156289E-17));
#7005=CARTESIAN_POINT('',(-0.173205080756888,-0.4,-2.12115047744981E-17));
#7006=CARTESIAN_POINT('',(-0.0866025403784438,-0.4,-0.15));
#7007=CARTESIAN_POINT('',(-0.173205080756888,-0.64,-2.77555756156289E-17));
#7008=CARTESIAN_POINT('',(-0.173205080756888,-0.4,-2.12115047744981E-17));
#7009=CARTESIAN_POINT('',(-0.0866025403784438,-0.64,-0.15));
#7010=CARTESIAN_POINT('Origin',(-0.0866025403784439,-0.4,0.15));
#7011=CARTESIAN_POINT('',(-0.0866025403784439,-0.4,0.15));
#7012=CARTESIAN_POINT('',(-0.173205080756888,-0.4,-2.12115047744981E-17));
#7013=CARTESIAN_POINT('',(-0.0866025403784439,-0.64,0.15));
#7014=CARTESIAN_POINT('',(-0.0866025403784439,-0.4,0.15));
#7015=CARTESIAN_POINT('',(-0.173205080756888,-0.64,-2.12115047744981E-17));
#7016=CARTESIAN_POINT('Origin',(0.0866025403784439,-0.4,0.15));
#7017=CARTESIAN_POINT('',(0.0866025403784439,-0.4,0.15));
#7018=CARTESIAN_POINT('',(-0.0866025403784439,-0.4,0.15));
#7019=CARTESIAN_POINT('',(0.0866025403784439,-0.64,0.15));
#7020=CARTESIAN_POINT('',(0.0866025403784439,-0.4,0.15));
#7021=CARTESIAN_POINT('',(-0.0866025403784439,-0.64,0.15));
#7022=CARTESIAN_POINT('Origin',(0.173205080756888,-0.4,0.));
#7023=CARTESIAN_POINT('',(0.0866025403784439,-0.4,0.15));
#7024=CARTESIAN_POINT('',(0.0866025403784439,-0.64,0.15));
#7025=CARTESIAN_POINT('Origin',(0.,-0.4,-2.77555756156289E-17));
#7026=CARTESIAN_POINT('Origin',(0.,-0.64,-2.77555756156289E-17));
#7027=CARTESIAN_POINT('',(0.,0.,0.));
#7028=CARTESIAN_POINT('',(0.,0.,0.));
#7029=CARTESIAN_POINT('',(0.,0.,0.));
#7030=CARTESIAN_POINT('',(0.,0.,0.));
#7031=CARTESIAN_POINT('',(0.,0.,0.));
#7032=CARTESIAN_POINT('',(0.,0.,0.));
#7033=CARTESIAN_POINT('',(0.,0.,0.));
#7034=CARTESIAN_POINT('',(0.,0.,0.));
#7035=CARTESIAN_POINT('',(0.,0.,0.));
#7036=CARTESIAN_POINT('',(0.,0.,0.));
#7037=CARTESIAN_POINT('',(0.,0.,0.));
#7038=CARTESIAN_POINT('',(0.,0.,0.));
#7039=CARTESIAN_POINT('',(0.,0.,0.));
#7040=CARTESIAN_POINT('',(0.,0.,0.));
#7041=CARTESIAN_POINT('',(0.,0.,0.));
#7042=CARTESIAN_POINT('',(-1.9,-3.,3.1));
#7043=CARTESIAN_POINT('',(-1.9,-3.1,3.1));
#7044=CARTESIAN_POINT('',(-1.9,3.,3.1));
#7045=CARTESIAN_POINT('',(-1.9,3.1,3.1));
#7046=CARTESIAN_POINT('',(-1.9,-3.,6.9));
#7047=CARTESIAN_POINT('',(-1.9,-3.1,6.9));
#7048=CARTESIAN_POINT('',(-1.9,3.,6.9));
#7049=CARTESIAN_POINT('',(-1.9,3.1,6.9));
#7050=CARTESIAN_POINT('',(1.9,-3.,3.1));
#7051=CARTESIAN_POINT('',(1.9,-3.1,3.1));
#7052=CARTESIAN_POINT('',(1.9,3.,3.1));
#7053=CARTESIAN_POINT('',(1.9,3.1,3.1));
#7054=CARTESIAN_POINT('',(1.9,-3.,6.9));
#7055=CARTESIAN_POINT('',(1.9,-3.1,6.9));
#7056=CARTESIAN_POINT('',(1.9,3.,6.9));
#7057=CARTESIAN_POINT('',(1.9,3.1,6.9));
#7058=CARTESIAN_POINT('',(0.,-4.35,5.));
#7059=CARTESIAN_POINT('',(0.,4.35,5.));
#7060=CARTESIAN_POINT('',(-1.3,-1.,8.5));
#7061=CARTESIAN_POINT('',(-1.3,1.,8.5));
#7062=CARTESIAN_POINT('',(1.3,-1.,8.5));
#7063=CARTESIAN_POINT('',(1.3,1.,8.5));
#7064=CARTESIAN_POINT('',(0.,0.,0.));
#7065=CARTESIAN_POINT('',(0.,0.,0.));
#7066=CARTESIAN_POINT('Origin',(-0.205,-0.205,6.));
#7067=CARTESIAN_POINT('',(0.205,-0.205,6.47171668469172));
#7068=CARTESIAN_POINT('',(-0.205,-0.205,6.47171668469172));
#7069=CARTESIAN_POINT('Origin',(0.,-0.205,5.));
#7070=CARTESIAN_POINT('',(0.205,-0.205,6.));
#7071=CARTESIAN_POINT('',(0.205,-0.205,6.));
#7072=CARTESIAN_POINT('',(-0.205,-0.205,6.));
#7073=CARTESIAN_POINT('',(-0.205,-0.205,6.));
#7074=CARTESIAN_POINT('',(-0.205,-0.205,6.));
#7075=CARTESIAN_POINT('Origin',(-0.205,0.205,6.));
#7076=CARTESIAN_POINT('',(-0.205,-2.51052593825207E-17,6.48592563743951));
#7077=CARTESIAN_POINT('Origin',(-0.205,0.,5.));
#7078=CARTESIAN_POINT('',(-0.205,0.205,6.));
#7079=CARTESIAN_POINT('',(-0.205,0.205,6.));
#7080=CARTESIAN_POINT('',(-0.205,0.205,6.47171668469172));
#7081=CARTESIAN_POINT('',(-0.205,0.205,6.));
#7082=CARTESIAN_POINT('Origin',(-0.205,0.,5.));
#7083=CARTESIAN_POINT('Origin',(0.205,0.205,6.));
#7084=CARTESIAN_POINT('',(0.205,0.205,6.47171668469172));
#7085=CARTESIAN_POINT('Origin',(0.,0.205,5.));
#7086=CARTESIAN_POINT('',(0.205,0.205,6.));
#7087=CARTESIAN_POINT('',(0.205,0.205,6.));
#7088=CARTESIAN_POINT('',(0.205,0.205,6.));
#7089=CARTESIAN_POINT('Origin',(0.205,-0.205,6.));
#7090=CARTESIAN_POINT('Origin',(0.205,0.,5.));
#7091=CARTESIAN_POINT('',(0.205,-0.205,6.));
#7092=CARTESIAN_POINT('Origin',(0.,0.,6.));
#7093=CARTESIAN_POINT('Origin',(0.,-1.6,5.));
#7094=CARTESIAN_POINT('',(-0.75,-1.29903810567666,5.));
#7095=CARTESIAN_POINT('Origin',(0.,-1.29903810567666,5.));
#7096=CARTESIAN_POINT('',(-0.75,1.29903810567666,5.));
#7097=CARTESIAN_POINT('',(-0.75,-1.6,5.));
#7098=CARTESIAN_POINT('Origin',(0.,1.29903810567666,5.));
#7099=CARTESIAN_POINT('Origin',(0.,0.,5.));
#7100=CARTESIAN_POINT('',(-9.18485099360515E-17,-1.12481983699639E-32,3.5));
#7101=CARTESIAN_POINT('Origin',(0.,0.,5.));
#7102=CARTESIAN_POINT('',(0.,0.,0.));
#7103=CARTESIAN_POINT('Origin',(0.,0.,8.5));
#7104=CARTESIAN_POINT('',(-0.165,-2.02066721859313E-17,8.5));
#7105=CARTESIAN_POINT('Origin',(0.,0.,8.5));
#7106=CARTESIAN_POINT('',(-0.165,2.02066721859313E-17,9.4));
#7107=CARTESIAN_POINT('',(-0.165,-2.02066721859313E-17,8.5));
#7108=CARTESIAN_POINT('Origin',(0.,0.,9.4));
#7109=CARTESIAN_POINT('Origin',(0.,0.,8.5));
#7110=CARTESIAN_POINT('Origin',(0.,0.,8.7));
#7111=CARTESIAN_POINT('',(-0.264575131106459,0.3,8.7));
#7112=CARTESIAN_POINT('',(-0.3,0.264575131106459,8.7));
#7113=CARTESIAN_POINT('Origin',(0.,0.,8.7));
#7114=CARTESIAN_POINT('',(-0.3,0.3,8.7));
#7115=CARTESIAN_POINT('',(-0.3,0.3,8.7));
#7116=CARTESIAN_POINT('',(0.3,0.3,8.7));
#7117=CARTESIAN_POINT('Origin',(0.,0.,8.7));
#7118=CARTESIAN_POINT('',(-0.3,-0.264575131106459,8.7));
#7119=CARTESIAN_POINT('',(-0.264575131106459,-0.3,8.7));
#7120=CARTESIAN_POINT('Origin',(0.,0.,8.7));
#7121=CARTESIAN_POINT('',(-0.3,-0.3,8.7));
#7122=CARTESIAN_POINT('',(-0.3,-0.3,8.7));
#7123=CARTESIAN_POINT('',(-0.3,0.3,8.7));
#7124=CARTESIAN_POINT('Origin',(0.,0.,8.7));
#7125=CARTESIAN_POINT('',(0.264575131106459,-0.3,8.7));
#7126=CARTESIAN_POINT('',(0.3,-0.264575131106459,8.7));
#7127=CARTESIAN_POINT('Origin',(0.,0.,8.7));
#7128=CARTESIAN_POINT('',(0.3,-0.3,8.7));
#7129=CARTESIAN_POINT('',(0.3,-0.3,8.7));
#7130=CARTESIAN_POINT('',(-0.3,-0.3,8.7));
#7131=CARTESIAN_POINT('Origin',(0.,0.,8.7));
#7132=CARTESIAN_POINT('',(0.3,0.264575131106459,8.7));
#7133=CARTESIAN_POINT('',(0.264575131106459,0.3,8.7));
#7134=CARTESIAN_POINT('Origin',(0.,0.,8.7));
#7135=CARTESIAN_POINT('',(0.3,0.3,8.7));
#7136=CARTESIAN_POINT('',(0.3,0.3,8.7));
#7137=CARTESIAN_POINT('',(0.3,-0.3,8.7));
#7138=CARTESIAN_POINT('Origin',(0.3,0.3,8.7));
#7139=CARTESIAN_POINT('',(0.15,0.3,8.7));
#7140=CARTESIAN_POINT('',(-0.3,0.3,9.4));
#7141=CARTESIAN_POINT('',(-0.3,0.3,8.7));
#7142=CARTESIAN_POINT('',(0.3,0.3,9.4));
#7143=CARTESIAN_POINT('',(0.3,0.3,9.4));
#7144=CARTESIAN_POINT('',(0.3,0.3,8.7));
#7145=CARTESIAN_POINT('Origin',(0.3,-0.3,8.7));
#7146=CARTESIAN_POINT('',(0.3,-0.15,8.7));
#7147=CARTESIAN_POINT('',(0.3,-0.3,9.4));
#7148=CARTESIAN_POINT('',(0.3,-0.3,9.4));
#7149=CARTESIAN_POINT('',(0.3,-0.3,8.7));
#7150=CARTESIAN_POINT('Origin',(-0.3,-0.3,8.7));
#7151=CARTESIAN_POINT('',(-0.15,-0.3,8.7));
#7152=CARTESIAN_POINT('',(-0.3,-0.3,9.4));
#7153=CARTESIAN_POINT('',(-0.3,-0.3,9.4));
#7154=CARTESIAN_POINT('',(-0.3,-0.3,8.7));
#7155=CARTESIAN_POINT('Origin',(-0.3,0.3,8.7));
#7156=CARTESIAN_POINT('',(-0.3,0.15,8.7));
#7157=CARTESIAN_POINT('',(-0.3,0.3,9.4));
#7158=CARTESIAN_POINT('Origin',(0.,0.,9.4));
#7159=CARTESIAN_POINT('Origin',(0.,0.,8.7));
#7160=CARTESIAN_POINT('Origin',(0.,0.,8.7));
#7161=CARTESIAN_POINT('Origin',(0.,0.,8.7));
#7162=CARTESIAN_POINT('',(-0.4,-4.89858719658941E-17,8.7));
#7163=CARTESIAN_POINT('Origin',(0.,0.,8.7));
#7164=CARTESIAN_POINT('Origin',(0.,0.,8.7));
#7165=CARTESIAN_POINT('Origin',(0.,0.,8.7));
#7166=CARTESIAN_POINT('Origin',(0.,0.,8.7));
#7167=CARTESIAN_POINT('Origin',(0.,0.,8.7));
#7168=CARTESIAN_POINT('Origin',(0.,0.,8.7));
#7169=CARTESIAN_POINT('Origin',(0.2,0.2,6.));
#7170=CARTESIAN_POINT('',(0.2,0.2,6.));
#7171=CARTESIAN_POINT('',(-0.2,0.2,6.));
#7172=CARTESIAN_POINT('',(0.2,0.2,6.));
#7173=CARTESIAN_POINT('',(-0.2,0.2,6.5));
#7174=CARTESIAN_POINT('',(-0.2,0.2,6.));
#7175=CARTESIAN_POINT('',(0.2,0.2,6.5));
#7176=CARTESIAN_POINT('',(0.1,0.2,6.5));
#7177=CARTESIAN_POINT('',(0.2,0.2,6.));
#7178=CARTESIAN_POINT('Origin',(0.2,-0.2,6.));
#7179=CARTESIAN_POINT('',(0.2,-0.2,6.));
#7180=CARTESIAN_POINT('',(0.2,-0.2,6.));
#7181=CARTESIAN_POINT('',(0.2,-0.2,6.5));
#7182=CARTESIAN_POINT('',(0.2,-0.1,6.5));
#7183=CARTESIAN_POINT('',(0.2,-0.2,6.));
#7184=CARTESIAN_POINT('Origin',(-0.2,-0.2,6.));
#7185=CARTESIAN_POINT('',(-0.2,-0.2,6.));
#7186=CARTESIAN_POINT('',(-0.2,-0.2,6.));
#7187=CARTESIAN_POINT('',(-0.2,-0.2,6.5));
#7188=CARTESIAN_POINT('',(-0.1,-0.2,6.5));
#7189=CARTESIAN_POINT('',(-0.2,-0.2,6.));
#7190=CARTESIAN_POINT('Origin',(-0.2,0.2,6.));
#7191=CARTESIAN_POINT('',(-0.2,0.2,6.));
#7192=CARTESIAN_POINT('',(-0.2,0.1,6.5));
#7193=CARTESIAN_POINT('Origin',(0.,0.,6.));
#7194=CARTESIAN_POINT('Origin',(0.,0.,6.5));
#7195=CARTESIAN_POINT('',(-0.4,-4.89858719658941E-17,6.5));
#7196=CARTESIAN_POINT('',(-0.4,-4.89858719658941E-17,6.5));
#7197=CARTESIAN_POINT('Origin',(0.,0.,6.5));
#7198=CARTESIAN_POINT('Origin',(0.,0.,6.5));
#7199=CARTESIAN_POINT('',(0.,0.,0.));
#7200=CARTESIAN_POINT('Origin',(-0.305,-0.305,8.9));
#7201=CARTESIAN_POINT('',(0.305,-0.305,9.4));
#7202=CARTESIAN_POINT('',(-0.305,-0.305,9.4));
#7203=CARTESIAN_POINT('',(1.6475,-0.305,9.4));
#7204=CARTESIAN_POINT('',(0.305,-0.305,9.));
#7205=CARTESIAN_POINT('',(0.305,-0.305,8.9));
#7206=CARTESIAN_POINT('',(-0.305,-0.305,9.));
#7207=CARTESIAN_POINT('',(1.6475,-0.305,9.));
#7208=CARTESIAN_POINT('',(-0.305,-0.305,8.9));
#7209=CARTESIAN_POINT('Origin',(-0.305,0.305,8.9));
#7210=CARTESIAN_POINT('',(-0.305,0.305,9.4));
#7211=CARTESIAN_POINT('',(-0.305,0.1525,9.4));
#7212=CARTESIAN_POINT('',(-0.305,0.305,9.));
#7213=CARTESIAN_POINT('',(-0.305,0.1525,9.));
#7214=CARTESIAN_POINT('',(-0.305,0.305,8.9));
#7215=CARTESIAN_POINT('Origin',(0.305,0.305,8.9));
#7216=CARTESIAN_POINT('',(0.305,0.305,9.4));
#7217=CARTESIAN_POINT('',(1.9525,0.305,9.4));
#7218=CARTESIAN_POINT('',(0.305,0.305,9.));
#7219=CARTESIAN_POINT('',(1.9525,0.305,9.));
#7220=CARTESIAN_POINT('',(0.305,0.305,8.9));
#7221=CARTESIAN_POINT('Origin',(0.305,-0.305,8.9));
#7222=CARTESIAN_POINT('',(0.305,-0.1525,9.4));
#7223=CARTESIAN_POINT('',(0.305,-0.1525,9.));
#7224=CARTESIAN_POINT('Origin',(8.,0.8,9.));
#7225=CARTESIAN_POINT('',(8.,0.8,9.));
#7226=CARTESIAN_POINT('',(-0.8,0.8,9.));
#7227=CARTESIAN_POINT('',(8.,0.8,9.));
#7228=CARTESIAN_POINT('',(-0.8,0.8,9.4));
#7229=CARTESIAN_POINT('',(-0.8,0.8,9.));
#7230=CARTESIAN_POINT('',(8.,0.8,9.4));
#7231=CARTESIAN_POINT('',(8.,0.8,9.4));
#7232=CARTESIAN_POINT('',(8.,0.8,9.));
#7233=CARTESIAN_POINT('Origin',(8.,-0.8,9.));
#7234=CARTESIAN_POINT('',(8.,-0.8,9.));
#7235=CARTESIAN_POINT('',(8.,-0.8,9.));
#7236=CARTESIAN_POINT('',(8.,-0.8,9.4));
#7237=CARTESIAN_POINT('',(8.,-0.8,9.4));
#7238=CARTESIAN_POINT('',(8.,-0.8,9.));
#7239=CARTESIAN_POINT('Origin',(-0.8,-0.8,9.));
#7240=CARTESIAN_POINT('',(-0.8,-0.8,9.));
#7241=CARTESIAN_POINT('',(-0.8,-0.8,9.));
#7242=CARTESIAN_POINT('',(-0.8,-0.8,9.4));
#7243=CARTESIAN_POINT('',(-0.8,-0.8,9.4));
#7244=CARTESIAN_POINT('',(-0.8,-0.8,9.));
#7245=CARTESIAN_POINT('Origin',(-0.8,0.8,9.));
#7246=CARTESIAN_POINT('',(-0.8,0.8,9.));
#7247=CARTESIAN_POINT('',(-0.8,0.8,9.4));
#7248=CARTESIAN_POINT('Origin',(3.6,0.,9.4));
#7249=CARTESIAN_POINT('Origin',(3.6,0.,9.));
#7250=CARTESIAN_POINT('',(0.,0.,0.));
#7251=CARTESIAN_POINT('Origin',(0.,0.,9.4));
#7252=CARTESIAN_POINT('',(-0.225,-2.75545529808154E-17,9.6));
#7253=CARTESIAN_POINT('Origin',(0.,0.,9.6));
#7254=CARTESIAN_POINT('',(-0.225,-2.75545529808154E-17,9.4));
#7255=CARTESIAN_POINT('',(-0.225,-2.75545529808154E-17,9.4));
#7256=CARTESIAN_POINT('Origin',(0.,0.,9.4));
#7257=CARTESIAN_POINT('Origin',(0.,0.,9.4));
#7258=CARTESIAN_POINT('',(-0.6,-7.34788079488412E-17,9.6));
#7259=CARTESIAN_POINT('Origin',(0.,0.,9.6));
#7260=CARTESIAN_POINT('',(-0.6,-7.34788079488412E-17,9.4));
#7261=CARTESIAN_POINT('',(-0.6,-7.34788079488412E-17,9.4));
#7262=CARTESIAN_POINT('Origin',(0.,0.,9.4));
#7263=CARTESIAN_POINT('Origin',(0.,0.,9.6));
#7264=CARTESIAN_POINT('Origin',(0.,0.,9.4));
#7265=CARTESIAN_POINT('',(0.,0.,0.));
#7266=CARTESIAN_POINT('Origin',(8.5,1.,9.4));
#7267=CARTESIAN_POINT('',(8.5,1.,9.4));
#7268=CARTESIAN_POINT('',(6.,1.,9.4));
#7269=CARTESIAN_POINT('',(8.5,1.,9.4));
#7270=CARTESIAN_POINT('',(6.,1.,10.2));
#7271=CARTESIAN_POINT('',(6.,1.,9.4));
#7272=CARTESIAN_POINT('',(8.5,1.,10.2));
#7273=CARTESIAN_POINT('',(8.5,1.,10.2));
#7274=CARTESIAN_POINT('',(8.5,1.,9.4));
#7275=CARTESIAN_POINT('Origin',(8.5,-1.,9.4));
#7276=CARTESIAN_POINT('',(8.5,-1.,9.4));
#7277=CARTESIAN_POINT('',(8.5,-1.,9.4));
#7278=CARTESIAN_POINT('',(8.5,-1.,10.2));
#7279=CARTESIAN_POINT('',(8.5,-1.,10.2));
#7280=CARTESIAN_POINT('',(8.5,-1.,9.4));
#7281=CARTESIAN_POINT('Origin',(6.,-1.,9.4));
#7282=CARTESIAN_POINT('',(6.,-1.,9.4));
#7283=CARTESIAN_POINT('',(6.,-1.,9.4));
#7284=CARTESIAN_POINT('',(6.,-1.,10.2));
#7285=CARTESIAN_POINT('',(6.,-1.,10.2));
#7286=CARTESIAN_POINT('',(6.,-1.,9.4));
#7287=CARTESIAN_POINT('Origin',(6.,1.,9.4));
#7288=CARTESIAN_POINT('',(6.,1.,9.4));
#7289=CARTESIAN_POINT('',(6.,1.,10.2));
#7290=CARTESIAN_POINT('Origin',(7.25,0.,10.2));
#7291=CARTESIAN_POINT('Origin',(7.25,0.,9.4));
#7292=CARTESIAN_POINT('',(0.,0.,0.));
#7293=CARTESIAN_POINT('Origin',(0.0866025403784439,-0.4,-0.15));
#7294=CARTESIAN_POINT('',(0.173205080756888,-0.4,0.));
#7295=CARTESIAN_POINT('',(0.0866025403784439,-0.4,-0.15));
#7296=CARTESIAN_POINT('',(0.173205080756888,-0.4,0.));
#7297=CARTESIAN_POINT('',(0.0866025403784439,-0.64,-0.15));
#7298=CARTESIAN_POINT('',(0.0866025403784439,-0.4,-0.15));
#7299=CARTESIAN_POINT('',(0.173205080756888,-0.64,0.));
#7300=CARTESIAN_POINT('',(0.173205080756888,-0.64,0.));
#7301=CARTESIAN_POINT('',(0.173205080756888,-0.4,0.));
#7302=CARTESIAN_POINT('Origin',(-0.0866025403784438,-0.4,-0.15));
#7303=CARTESIAN_POINT('',(-0.0866025403784438,-0.4,-0.15));
#7304=CARTESIAN_POINT('',(0.0866025403784439,-0.4,-0.15));
#7305=CARTESIAN_POINT('',(-0.0866025403784438,-0.64,-0.15));
#7306=CARTESIAN_POINT('',(-0.0866025403784438,-0.4,-0.15));
#7307=CARTESIAN_POINT('',(0.0866025403784439,-0.64,-0.15));
#7308=CARTESIAN_POINT('Origin',(-0.173205080756888,-0.4,-2.77555756156289E-17));
#7309=CARTESIAN_POINT('',(-0.173205080756888,-0.4,-2.12115047744981E-17));
#7310=CARTESIAN_POINT('',(-0.0866025403784438,-0.4,-0.15));
#7311=CARTESIAN_POINT('',(-0.173205080756888,-0.64,-2.77555756156289E-17));
#7312=CARTESIAN_POINT('',(-0.173205080756888,-0.4,-2.12115047744981E-17));
#7313=CARTESIAN_POINT('',(-0.0866025403784438,-0.64,-0.15));
#7314=CARTESIAN_POINT('Origin',(-0.0866025403784439,-0.4,0.15));
#7315=CARTESIAN_POINT('',(-0.0866025403784439,-0.4,0.15));
#7316=CARTESIAN_POINT('',(-0.173205080756888,-0.4,-2.12115047744981E-17));
#7317=CARTESIAN_POINT('',(-0.0866025403784439,-0.64,0.15));
#7318=CARTESIAN_POINT('',(-0.0866025403784439,-0.4,0.15));
#7319=CARTESIAN_POINT('',(-0.173205080756888,-0.64,-2.12115047744981E-17));
#7320=CARTESIAN_POINT('Origin',(0.0866025403784439,-0.4,0.15));
#7321=CARTESIAN_POINT('',(0.0866025403784439,-0.4,0.15));
#7322=CARTESIAN_POINT('',(-0.0866025403784439,-0.4,0.15));
#7323=CARTESIAN_POINT('',(0.0866025403784439,-0.64,0.15));
#7324=CARTESIAN_POINT('',(0.0866025403784439,-0.4,0.15));
#7325=CARTESIAN_POINT('',(-0.0866025403784439,-0.64,0.15));
#7326=CARTESIAN_POINT('Origin',(0.173205080756888,-0.4,0.));
#7327=CARTESIAN_POINT('',(0.0866025403784439,-0.4,0.15));
#7328=CARTESIAN_POINT('',(0.0866025403784439,-0.64,0.15));
#7329=CARTESIAN_POINT('Origin',(0.,-0.4,-2.77555756156289E-17));
#7330=CARTESIAN_POINT('Origin',(0.,-0.64,-2.77555756156289E-17));
#7331=CARTESIAN_POINT('Origin',(0.,-1.,0.));
#7332=CARTESIAN_POINT('',(-0.1954,-1.,2.39295984553393E-17));
#7333=CARTESIAN_POINT('Origin',(0.,-1.,0.));
#7334=CARTESIAN_POINT('Origin',(0.3,0.4,0.));
#7335=CARTESIAN_POINT('',(-0.3,0.4,-3.67394039744206E-17));
#7336=CARTESIAN_POINT('Origin',(0.,0.4,0.));
#7337=CARTESIAN_POINT('Origin',(0.,0.375,0.));
#7338=CARTESIAN_POINT('',(-0.35,0.35,-4.28626379701573E-17));
#7339=CARTESIAN_POINT('Origin',(0.,0.35,0.));
#7340=CARTESIAN_POINT('',(-0.325,0.375,-3.9801020972289E-17));
#7341=CARTESIAN_POINT('Origin',(0.,0.19,0.));
#7342=CARTESIAN_POINT('',(-0.35,0.03,-4.28626379701574E-17));
#7343=CARTESIAN_POINT('Origin',(0.,0.03,0.));
#7344=CARTESIAN_POINT('',(-0.35,0.19,-4.28626379701574E-17));
#7345=CARTESIAN_POINT('Origin',(0.,0.0149999999999999,0.));
#7346=CARTESIAN_POINT('',(-0.32,-3.29597460435593E-17,-3.91886975727153E-17));
#7347=CARTESIAN_POINT('Origin',(0.,0.,0.));
#7348=CARTESIAN_POINT('',(-0.335,0.0149999999999999,-4.10256677714363E-17));
#7349=CARTESIAN_POINT('Origin',(0.22,0.,0.));
#7350=CARTESIAN_POINT('',(-0.22,-6.93889390390723E-18,-2.69422295812418E-17));
#7351=CARTESIAN_POINT('Origin',(0.,0.,0.));
#7352=CARTESIAN_POINT('Origin',(0.,-0.02,0.));
#7353=CARTESIAN_POINT('',(-0.1954,-0.0492,2.39295984553393E-17));
#7354=CARTESIAN_POINT('Origin',(0.,-0.0492,0.));
#7355=CARTESIAN_POINT('',(-0.21,-0.02,-2.57175827820944E-17));
#7356=CARTESIAN_POINT('Origin',(0.,-0.8,0.));
#7357=CARTESIAN_POINT('',(-0.1954,-0.8,-2.39295984553393E-17));
#7358=CARTESIAN_POINT('',(0.,0.,0.));
#7359=CARTESIAN_POINT('',(0.,0.,0.));
#7360=CARTESIAN_POINT('',(0.,0.,0.));
#7361=CARTESIAN_POINT('',(0.,0.,0.));
#7362=CARTESIAN_POINT('',(0.,0.,0.));
#7363=CARTESIAN_POINT('',(0.,0.,9.6));
#7364=CARTESIAN_POINT('',(0.,0.,0.));
#7365=CARTESIAN_POINT('',(0.,0.,0.));
#7366=UNCERTAINTY_MEASURE_WITH_UNIT(LENGTH_MEASURE(0.001),#7426,
'DISTANCE_ACCURACY_VALUE',
'Maximum model space distance between geometric entities at asserted c
onnectivities');
#7367=UNCERTAINTY_MEASURE_WITH_UNIT(LENGTH_MEASURE(0.001),#7426,
'DISTANCE_ACCURACY_VALUE',
'Maximum model space distance between geometric entities at asserted c
onnectivities');
#7368=UNCERTAINTY_MEASURE_WITH_UNIT(LENGTH_MEASURE(0.001),#7426,
'DISTANCE_ACCURACY_VALUE',
'Maximum model space distance between geometric entities at asserted c
onnectivities');
#7369=UNCERTAINTY_MEASURE_WITH_UNIT(LENGTH_MEASURE(0.001),#7426,
'DISTANCE_ACCURACY_VALUE',
'Maximum model space distance between geometric entities at asserted c
onnectivities');
#7370=UNCERTAINTY_MEASURE_WITH_UNIT(LENGTH_MEASURE(0.001),#7426,
'DISTANCE_ACCURACY_VALUE',
'Maximum model space distance between geometric entities at asserted c
onnectivities');
#7371=UNCERTAINTY_MEASURE_WITH_UNIT(LENGTH_MEASURE(0.001),#7426,
'DISTANCE_ACCURACY_VALUE',
'Maximum model space distance between geometric entities at asserted c
onnectivities');
#7372=UNCERTAINTY_MEASURE_WITH_UNIT(LENGTH_MEASURE(0.001),#7426,
'DISTANCE_ACCURACY_VALUE',
'Maximum model space distance between geometric entities at asserted c
onnectivities');
#7373=UNCERTAINTY_MEASURE_WITH_UNIT(LENGTH_MEASURE(0.001),#7426,
'DISTANCE_ACCURACY_VALUE',
'Maximum model space distance between geometric entities at asserted c
onnectivities');
#7374=UNCERTAINTY_MEASURE_WITH_UNIT(LENGTH_MEASURE(0.001),#7426,
'DISTANCE_ACCURACY_VALUE',
'Maximum model space distance between geometric entities at asserted c
onnectivities');
#7375=UNCERTAINTY_MEASURE_WITH_UNIT(LENGTH_MEASURE(0.001),#7426,
'DISTANCE_ACCURACY_VALUE',
'Maximum model space distance between geometric entities at asserted c
onnectivities');
#7376=UNCERTAINTY_MEASURE_WITH_UNIT(LENGTH_MEASURE(0.001),#7426,
'DISTANCE_ACCURACY_VALUE',
'Maximum model space distance between geometric entities at asserted c
onnectivities');
#7377=UNCERTAINTY_MEASURE_WITH_UNIT(LENGTH_MEASURE(0.001),#7426,
'DISTANCE_ACCURACY_VALUE',
'Maximum model space distance between geometric entities at asserted c
onnectivities');
#7378=UNCERTAINTY_MEASURE_WITH_UNIT(LENGTH_MEASURE(0.001),#7426,
'DISTANCE_ACCURACY_VALUE',
'Maximum model space distance between geometric entities at asserted c
onnectivities');
#7379=UNCERTAINTY_MEASURE_WITH_UNIT(LENGTH_MEASURE(0.001),#7426,
'DISTANCE_ACCURACY_VALUE',
'Maximum model space distance between geometric entities at asserted c
onnectivities');
#7380=UNCERTAINTY_MEASURE_WITH_UNIT(LENGTH_MEASURE(0.001),#7426,
'DISTANCE_ACCURACY_VALUE',
'Maximum model space distance between geometric entities at asserted c
onnectivities');
#7381=UNCERTAINTY_MEASURE_WITH_UNIT(LENGTH_MEASURE(0.001),#7426,
'DISTANCE_ACCURACY_VALUE',
'Maximum model space distance between geometric entities at asserted c
onnectivities');
#7382=UNCERTAINTY_MEASURE_WITH_UNIT(LENGTH_MEASURE(0.001),#7426,
'DISTANCE_ACCURACY_VALUE',
'Maximum model space distance between geometric entities at asserted c
onnectivities');
#7383=UNCERTAINTY_MEASURE_WITH_UNIT(LENGTH_MEASURE(0.001),#7426,
'DISTANCE_ACCURACY_VALUE',
'Maximum model space distance between geometric entities at asserted c
onnectivities');
#7384=UNCERTAINTY_MEASURE_WITH_UNIT(LENGTH_MEASURE(0.001),#7426,
'DISTANCE_ACCURACY_VALUE',
'Maximum model space distance between geometric entities at asserted c
onnectivities');
#7385=UNCERTAINTY_MEASURE_WITH_UNIT(LENGTH_MEASURE(0.001),#7426,
'DISTANCE_ACCURACY_VALUE',
'Maximum model space distance between geometric entities at asserted c
onnectivities');
#7386=UNCERTAINTY_MEASURE_WITH_UNIT(LENGTH_MEASURE(0.001),#7426,
'DISTANCE_ACCURACY_VALUE',
'Maximum model space distance between geometric entities at asserted c
onnectivities');
#7387=UNCERTAINTY_MEASURE_WITH_UNIT(LENGTH_MEASURE(0.001),#7426,
'DISTANCE_ACCURACY_VALUE',
'Maximum model space distance between geometric entities at asserted c
onnectivities');
#7388=UNCERTAINTY_MEASURE_WITH_UNIT(LENGTH_MEASURE(0.001),#7426,
'DISTANCE_ACCURACY_VALUE',
'Maximum model space distance between geometric entities at asserted c
onnectivities');
#7389=UNCERTAINTY_MEASURE_WITH_UNIT(LENGTH_MEASURE(0.001),#7426,
'DISTANCE_ACCURACY_VALUE',
'Maximum model space distance between geometric entities at asserted c
onnectivities');
#7390=UNCERTAINTY_MEASURE_WITH_UNIT(LENGTH_MEASURE(0.001),#7426,
'DISTANCE_ACCURACY_VALUE',
'Maximum model space distance between geometric entities at asserted c
onnectivities');
#7391=UNCERTAINTY_MEASURE_WITH_UNIT(LENGTH_MEASURE(0.001),#7426,
'DISTANCE_ACCURACY_VALUE',
'Maximum model space distance between geometric entities at asserted c
onnectivities');
#7392=UNCERTAINTY_MEASURE_WITH_UNIT(LENGTH_MEASURE(0.001),#7426,
'DISTANCE_ACCURACY_VALUE',
'Maximum model space distance between geometric entities at asserted c
onnectivities');
#7393=UNCERTAINTY_MEASURE_WITH_UNIT(LENGTH_MEASURE(0.001),#7426,
'DISTANCE_ACCURACY_VALUE',
'Maximum model space distance between geometric entities at asserted c
onnectivities');
#7394=UNCERTAINTY_MEASURE_WITH_UNIT(LENGTH_MEASURE(0.001),#7426,
'DISTANCE_ACCURACY_VALUE',
'Maximum model space distance between geometric entities at asserted c
onnectivities');
#7395=UNCERTAINTY_MEASURE_WITH_UNIT(LENGTH_MEASURE(0.001),#7426,
'DISTANCE_ACCURACY_VALUE',
'Maximum model space distance between geometric entities at asserted c
onnectivities');
#7396=(
GEOMETRIC_REPRESENTATION_CONTEXT(3)
GLOBAL_UNCERTAINTY_ASSIGNED_CONTEXT((#7366))
GLOBAL_UNIT_ASSIGNED_CONTEXT((#7426,#7428,#7429))
REPRESENTATION_CONTEXT('','3D')
);
#7397=(
GEOMETRIC_REPRESENTATION_CONTEXT(3)
GLOBAL_UNCERTAINTY_ASSIGNED_CONTEXT((#7367))
GLOBAL_UNIT_ASSIGNED_CONTEXT((#7426,#7428,#7429))
REPRESENTATION_CONTEXT('','3D')
);
#7398=(
GEOMETRIC_REPRESENTATION_CONTEXT(3)
GLOBAL_UNCERTAINTY_ASSIGNED_CONTEXT((#7368))
GLOBAL_UNIT_ASSIGNED_CONTEXT((#7426,#7428,#7429))
REPRESENTATION_CONTEXT('','3D')
);
#7399=(
GEOMETRIC_REPRESENTATION_CONTEXT(3)
GLOBAL_UNCERTAINTY_ASSIGNED_CONTEXT((#7369))
GLOBAL_UNIT_ASSIGNED_CONTEXT((#7426,#7428,#7429))
REPRESENTATION_CONTEXT('','3D')
);
#7400=(
GEOMETRIC_REPRESENTATION_CONTEXT(3)
GLOBAL_UNCERTAINTY_ASSIGNED_CONTEXT((#7370))
GLOBAL_UNIT_ASSIGNED_CONTEXT((#7426,#7428,#7429))
REPRESENTATION_CONTEXT('','3D')
);
#7401=(
GEOMETRIC_REPRESENTATION_CONTEXT(3)
GLOBAL_UNCERTAINTY_ASSIGNED_CONTEXT((#7371))
GLOBAL_UNIT_ASSIGNED_CONTEXT((#7426,#7428,#7429))
REPRESENTATION_CONTEXT('','3D')
);
#7402=(
GEOMETRIC_REPRESENTATION_CONTEXT(3)
GLOBAL_UNCERTAINTY_ASSIGNED_CONTEXT((#7372))
GLOBAL_UNIT_ASSIGNED_CONTEXT((#7426,#7428,#7429))
REPRESENTATION_CONTEXT('','3D')
);
#7403=(
GEOMETRIC_REPRESENTATION_CONTEXT(3)
GLOBAL_UNCERTAINTY_ASSIGNED_CONTEXT((#7373))
GLOBAL_UNIT_ASSIGNED_CONTEXT((#7426,#7428,#7429))
REPRESENTATION_CONTEXT('','3D')
);
#7404=(
GEOMETRIC_REPRESENTATION_CONTEXT(3)
GLOBAL_UNCERTAINTY_ASSIGNED_CONTEXT((#7374))
GLOBAL_UNIT_ASSIGNED_CONTEXT((#7426,#7428,#7429))
REPRESENTATION_CONTEXT('','3D')
);
#7405=(
GEOMETRIC_REPRESENTATION_CONTEXT(3)
GLOBAL_UNCERTAINTY_ASSIGNED_CONTEXT((#7375))
GLOBAL_UNIT_ASSIGNED_CONTEXT((#7426,#7428,#7429))
REPRESENTATION_CONTEXT('','3D')
);
#7406=(
GEOMETRIC_REPRESENTATION_CONTEXT(3)
GLOBAL_UNCERTAINTY_ASSIGNED_CONTEXT((#7376))
GLOBAL_UNIT_ASSIGNED_CONTEXT((#7426,#7428,#7429))
REPRESENTATION_CONTEXT('','3D')
);
#7407=(
GEOMETRIC_REPRESENTATION_CONTEXT(3)
GLOBAL_UNCERTAINTY_ASSIGNED_CONTEXT((#7377))
GLOBAL_UNIT_ASSIGNED_CONTEXT((#7426,#7428,#7429))
REPRESENTATION_CONTEXT('','3D')
);
#7408=(
GEOMETRIC_REPRESENTATION_CONTEXT(3)
GLOBAL_UNCERTAINTY_ASSIGNED_CONTEXT((#7378))
GLOBAL_UNIT_ASSIGNED_CONTEXT((#7426,#7428,#7429))
REPRESENTATION_CONTEXT('','3D')
);
#7409=(
GEOMETRIC_REPRESENTATION_CONTEXT(3)
GLOBAL_UNCERTAINTY_ASSIGNED_CONTEXT((#7379))
GLOBAL_UNIT_ASSIGNED_CONTEXT((#7426,#7428,#7429))
REPRESENTATION_CONTEXT('','3D')
);
#7410=(
GEOMETRIC_REPRESENTATION_CONTEXT(3)
GLOBAL_UNCERTAINTY_ASSIGNED_CONTEXT((#7380))
GLOBAL_UNIT_ASSIGNED_CONTEXT((#7426,#7428,#7429))
REPRESENTATION_CONTEXT('','3D')
);
#7411=(
GEOMETRIC_REPRESENTATION_CONTEXT(3)
GLOBAL_UNCERTAINTY_ASSIGNED_CONTEXT((#7381))
GLOBAL_UNIT_ASSIGNED_CONTEXT((#7426,#7428,#7429))
REPRESENTATION_CONTEXT('','3D')
);
#7412=(
GEOMETRIC_REPRESENTATION_CONTEXT(3)
GLOBAL_UNCERTAINTY_ASSIGNED_CONTEXT((#7382))
GLOBAL_UNIT_ASSIGNED_CONTEXT((#7426,#7428,#7429))
REPRESENTATION_CONTEXT('','3D')
);
#7413=(
GEOMETRIC_REPRESENTATION_CONTEXT(3)
GLOBAL_UNCERTAINTY_ASSIGNED_CONTEXT((#7383))
GLOBAL_UNIT_ASSIGNED_CONTEXT((#7426,#7428,#7429))
REPRESENTATION_CONTEXT('','3D')
);
#7414=(
GEOMETRIC_REPRESENTATION_CONTEXT(3)
GLOBAL_UNCERTAINTY_ASSIGNED_CONTEXT((#7384))
GLOBAL_UNIT_ASSIGNED_CONTEXT((#7426,#7428,#7429))
REPRESENTATION_CONTEXT('','3D')
);
#7415=(
GEOMETRIC_REPRESENTATION_CONTEXT(3)
GLOBAL_UNCERTAINTY_ASSIGNED_CONTEXT((#7385))
GLOBAL_UNIT_ASSIGNED_CONTEXT((#7426,#7428,#7429))
REPRESENTATION_CONTEXT('','3D')
);
#7416=(
GEOMETRIC_REPRESENTATION_CONTEXT(3)
GLOBAL_UNCERTAINTY_ASSIGNED_CONTEXT((#7386))
GLOBAL_UNIT_ASSIGNED_CONTEXT((#7426,#7428,#7429))
REPRESENTATION_CONTEXT('','3D')
);
#7417=(
GEOMETRIC_REPRESENTATION_CONTEXT(3)
GLOBAL_UNCERTAINTY_ASSIGNED_CONTEXT((#7387))
GLOBAL_UNIT_ASSIGNED_CONTEXT((#7426,#7428,#7429))
REPRESENTATION_CONTEXT('','3D')
);
#7418=(
GEOMETRIC_REPRESENTATION_CONTEXT(3)
GLOBAL_UNCERTAINTY_ASSIGNED_CONTEXT((#7388))
GLOBAL_UNIT_ASSIGNED_CONTEXT((#7426,#7428,#7429))
REPRESENTATION_CONTEXT('','3D')
);
#7419=(
GEOMETRIC_REPRESENTATION_CONTEXT(3)
GLOBAL_UNCERTAINTY_ASSIGNED_CONTEXT((#7389))
GLOBAL_UNIT_ASSIGNED_CONTEXT((#7426,#7428,#7429))
REPRESENTATION_CONTEXT('','3D')
);
#7420=(
GEOMETRIC_REPRESENTATION_CONTEXT(3)
GLOBAL_UNCERTAINTY_ASSIGNED_CONTEXT((#7390))
GLOBAL_UNIT_ASSIGNED_CONTEXT((#7426,#7428,#7429))
REPRESENTATION_CONTEXT('','3D')
);
#7421=(
GEOMETRIC_REPRESENTATION_CONTEXT(3)
GLOBAL_UNCERTAINTY_ASSIGNED_CONTEXT((#7391))
GLOBAL_UNIT_ASSIGNED_CONTEXT((#7426,#7428,#7429))
REPRESENTATION_CONTEXT('','3D')
);
#7422=(
GEOMETRIC_REPRESENTATION_CONTEXT(3)
GLOBAL_UNCERTAINTY_ASSIGNED_CONTEXT((#7392))
GLOBAL_UNIT_ASSIGNED_CONTEXT((#7426,#7428,#7429))
REPRESENTATION_CONTEXT('','3D')
);
#7423=(
GEOMETRIC_REPRESENTATION_CONTEXT(3)
GLOBAL_UNCERTAINTY_ASSIGNED_CONTEXT((#7393))
GLOBAL_UNIT_ASSIGNED_CONTEXT((#7426,#7428,#7429))
REPRESENTATION_CONTEXT('','3D')
);
#7424=(
GEOMETRIC_REPRESENTATION_CONTEXT(3)
GLOBAL_UNCERTAINTY_ASSIGNED_CONTEXT((#7394))
GLOBAL_UNIT_ASSIGNED_CONTEXT((#7426,#7428,#7429))
REPRESENTATION_CONTEXT('','3D')
);
#7425=(
GEOMETRIC_REPRESENTATION_CONTEXT(3)
GLOBAL_UNCERTAINTY_ASSIGNED_CONTEXT((#7395))
GLOBAL_UNIT_ASSIGNED_CONTEXT((#7426,#7428,#7429))
REPRESENTATION_CONTEXT('','3D')
);
#7426=(
LENGTH_UNIT()
NAMED_UNIT(*)
SI_UNIT(.CENTI.,.METRE.)
);
#7427=(
LENGTH_UNIT()
NAMED_UNIT(*)
SI_UNIT($,.METRE.)
);
#7428=(
NAMED_UNIT(*)
PLANE_ANGLE_UNIT()
SI_UNIT($,.RADIAN.)
);
#7429=(
NAMED_UNIT(*)
SI_UNIT($,.STERADIAN.)
SOLID_ANGLE_UNIT()
);
#7430=SHAPE_DEFINITION_REPRESENTATION(#7459,#7533);
#7431=SHAPE_DEFINITION_REPRESENTATION(#7460,#7534);
#7432=SHAPE_DEFINITION_REPRESENTATION(#7461,#7535);
#7433=SHAPE_DEFINITION_REPRESENTATION(#7462,#7536);
#7434=SHAPE_DEFINITION_REPRESENTATION(#7463,#7537);
#7435=SHAPE_DEFINITION_REPRESENTATION(#7464,#7538);
#7436=SHAPE_DEFINITION_REPRESENTATION(#7465,#7539);
#7437=SHAPE_DEFINITION_REPRESENTATION(#7466,#7540);
#7438=SHAPE_DEFINITION_REPRESENTATION(#7467,#7541);
#7439=SHAPE_DEFINITION_REPRESENTATION(#7468,#7542);
#7440=SHAPE_DEFINITION_REPRESENTATION(#7469,#7543);
#7441=SHAPE_DEFINITION_REPRESENTATION(#7470,#7544);
#7442=SHAPE_DEFINITION_REPRESENTATION(#7471,#7545);
#7443=SHAPE_DEFINITION_REPRESENTATION(#7472,#7546);
#7444=SHAPE_DEFINITION_REPRESENTATION(#7473,#7547);
#7445=SHAPE_DEFINITION_REPRESENTATION(#7474,#7548);
#7446=SHAPE_DEFINITION_REPRESENTATION(#7475,#7549);
#7447=SHAPE_DEFINITION_REPRESENTATION(#7476,#7550);
#7448=SHAPE_DEFINITION_REPRESENTATION(#7477,#7551);
#7449=SHAPE_DEFINITION_REPRESENTATION(#7478,#7552);
#7450=SHAPE_DEFINITION_REPRESENTATION(#7479,#7553);
#7451=SHAPE_DEFINITION_REPRESENTATION(#7480,#7554);
#7452=SHAPE_DEFINITION_REPRESENTATION(#7518,#7555);
#7453=SHAPE_DEFINITION_REPRESENTATION(#7519,#7556);
#7454=SHAPE_DEFINITION_REPRESENTATION(#7520,#7557);
#7455=SHAPE_DEFINITION_REPRESENTATION(#7521,#7558);
#7456=SHAPE_DEFINITION_REPRESENTATION(#7522,#7559);
#7457=SHAPE_DEFINITION_REPRESENTATION(#7523,#7560);
#7458=SHAPE_DEFINITION_REPRESENTATION(#7524,#7561);
#7459=PRODUCT_DEFINITION_SHAPE('',$,#7563);
#7460=PRODUCT_DEFINITION_SHAPE('',$,#7564);
#7461=PRODUCT_DEFINITION_SHAPE('',$,#7565);
#7462=PRODUCT_DEFINITION_SHAPE('',$,#7566);
#7463=PRODUCT_DEFINITION_SHAPE('',$,#7567);
#7464=PRODUCT_DEFINITION_SHAPE('',$,#7568);
#7465=PRODUCT_DEFINITION_SHAPE('',$,#7569);
#7466=PRODUCT_DEFINITION_SHAPE('',$,#7570);
#7467=PRODUCT_DEFINITION_SHAPE('',$,#7571);
#7468=PRODUCT_DEFINITION_SHAPE('',$,#7572);
#7469=PRODUCT_DEFINITION_SHAPE('',$,#7573);
#7470=PRODUCT_DEFINITION_SHAPE('',$,#7574);
#7471=PRODUCT_DEFINITION_SHAPE('',$,#7575);
#7472=PRODUCT_DEFINITION_SHAPE('',$,#7576);
#7473=PRODUCT_DEFINITION_SHAPE('',$,#7577);
#7474=PRODUCT_DEFINITION_SHAPE('',$,#7578);
#7475=PRODUCT_DEFINITION_SHAPE('',$,#7579);
#7476=PRODUCT_DEFINITION_SHAPE('',$,#7580);
#7477=PRODUCT_DEFINITION_SHAPE('',$,#7581);
#7478=PRODUCT_DEFINITION_SHAPE('',$,#7582);
#7479=PRODUCT_DEFINITION_SHAPE('',$,#7583);
#7480=PRODUCT_DEFINITION_SHAPE('',$,#7584);
#7481=PRODUCT_DEFINITION_SHAPE($,$,#146);
#7482=PRODUCT_DEFINITION_SHAPE($,$,#147);
#7483=PRODUCT_DEFINITION_SHAPE($,$,#148);
#7484=PRODUCT_DEFINITION_SHAPE($,$,#149);
#7485=PRODUCT_DEFINITION_SHAPE($,$,#150);
#7486=PRODUCT_DEFINITION_SHAPE($,$,#151);
#7487=PRODUCT_DEFINITION_SHAPE($,$,#152);
#7488=PRODUCT_DEFINITION_SHAPE($,$,#153);
#7489=PRODUCT_DEFINITION_SHAPE($,$,#154);
#7490=PRODUCT_DEFINITION_SHAPE($,$,#155);
#7491=PRODUCT_DEFINITION_SHAPE($,$,#156);
#7492=PRODUCT_DEFINITION_SHAPE($,$,#157);
#7493=PRODUCT_DEFINITION_SHAPE($,$,#158);
#7494=PRODUCT_DEFINITION_SHAPE($,$,#159);
#7495=PRODUCT_DEFINITION_SHAPE($,$,#160);
#7496=PRODUCT_DEFINITION_SHAPE($,$,#161);
#7497=PRODUCT_DEFINITION_SHAPE($,$,#162);
#7498=PRODUCT_DEFINITION_SHAPE($,$,#163);
#7499=PRODUCT_DEFINITION_SHAPE($,$,#164);
#7500=PRODUCT_DEFINITION_SHAPE($,$,#165);
#7501=PRODUCT_DEFINITION_SHAPE($,$,#166);
#7502=PRODUCT_DEFINITION_SHAPE($,$,#167);
#7503=PRODUCT_DEFINITION_SHAPE($,$,#168);
#7504=PRODUCT_DEFINITION_SHAPE($,$,#169);
#7505=PRODUCT_DEFINITION_SHAPE($,$,#170);
#7506=PRODUCT_DEFINITION_SHAPE($,$,#171);
#7507=PRODUCT_DEFINITION_SHAPE($,$,#172);
#7508=PRODUCT_DEFINITION_SHAPE($,$,#173);
#7509=PRODUCT_DEFINITION_SHAPE($,$,#174);
#7510=PRODUCT_DEFINITION_SHAPE($,$,#175);
#7511=PRODUCT_DEFINITION_SHAPE($,$,#176);
#7512=PRODUCT_DEFINITION_SHAPE($,$,#177);
#7513=PRODUCT_DEFINITION_SHAPE($,$,#178);
#7514=PRODUCT_DEFINITION_SHAPE($,$,#179);
#7515=PRODUCT_DEFINITION_SHAPE($,$,#180);
#7516=PRODUCT_DEFINITION_SHAPE($,$,#181);
#7517=PRODUCT_DEFINITION_SHAPE($,$,#182);
#7518=PRODUCT_DEFINITION_SHAPE('',$,#7585);
#7519=PRODUCT_DEFINITION_SHAPE('',$,#7586);
#7520=PRODUCT_DEFINITION_SHAPE('',$,#7587);
#7521=PRODUCT_DEFINITION_SHAPE('',$,#7588);
#7522=PRODUCT_DEFINITION_SHAPE('',$,#7589);
#7523=PRODUCT_DEFINITION_SHAPE('',$,#7590);
#7524=PRODUCT_DEFINITION_SHAPE('',$,#7591);
#7525=PRODUCT_DEFINITION_SHAPE($,$,#183);
#7526=PRODUCT_DEFINITION_SHAPE($,$,#184);
#7527=PRODUCT_DEFINITION_SHAPE($,$,#185);
#7528=PRODUCT_DEFINITION_SHAPE($,$,#186);
#7529=PRODUCT_DEFINITION_SHAPE($,$,#187);
#7530=PRODUCT_DEFINITION_SHAPE($,$,#188);
#7531=PRODUCT_DEFINITION_SHAPE($,$,#189);
#7532=PRODUCT_DEFINITION_SHAPE($,$,#190);
#7533=SHAPE_REPRESENTATION('',(#4398,#4894,#4895),#7396);
#7534=SHAPE_REPRESENTATION('',(#4399,#4748,#4749,#4750,#4751,#4752,#4753,
#4754,#4755,#4756,#4757,#4758,#4759,#4760,#4761,#4762,#4763,#4764,#4765,
#4766,#4767,#4768,#4769,#4770,#4771,#4772,#4773,#4774,#4775,#4776,#4777,
#4778,#4779,#4780,#4781,#4782,#4783,#4784),#7397);
#7535=SHAPE_REPRESENTATION('',(#4400),#7398);
#7536=SHAPE_REPRESENTATION('',(#4443),#7399);
#7537=SHAPE_REPRESENTATION('',(#4454),#7400);
#7538=SHAPE_REPRESENTATION('',(#4497),#7401);
#7539=SHAPE_REPRESENTATION('',(#4508),#7402);
#7540=SHAPE_REPRESENTATION('',(#4535),#7403);
#7541=SHAPE_REPRESENTATION('',(#4548),#7404);
#7542=SHAPE_REPRESENTATION('',(#4552),#7405);
#7543=SHAPE_REPRESENTATION('',(#4565),#7406);
#7544=SHAPE_REPRESENTATION('',(#4595),#7407);
#7545=SHAPE_REPRESENTATION('',(#4604),#7408);
#7546=SHAPE_REPRESENTATION('',(#4613),#7409);
#7547=SHAPE_REPRESENTATION('',(#4622),#7410);
#7548=SHAPE_REPRESENTATION('',(#4631),#7411);
#7549=SHAPE_REPRESENTATION('',(#4637),#7412);
#7550=SHAPE_REPRESENTATION('',(#4643),#7413);
#7551=SHAPE_REPRESENTATION('',(#4671),#7414);
#7552=SHAPE_REPRESENTATION('',(#4682),#7415);
#7553=SHAPE_REPRESENTATION('',(#4698),#7416);
#7554=SHAPE_REPRESENTATION('',(#4722),#7417);
#7555=SHAPE_REPRESENTATION('',(#4785,#4888,#4889,#4890,#4891,#4892,#4893),
#7418);
#7556=SHAPE_REPRESENTATION('',(#4786),#7419);
#7557=SHAPE_REPRESENTATION('',(#4802),#7420);
#7558=SHAPE_REPRESENTATION('',(#4837),#7421);
#7559=SHAPE_REPRESENTATION('',(#4848),#7422);
#7560=SHAPE_REPRESENTATION('',(#4857),#7423);
#7561=SHAPE_REPRESENTATION('',(#4864),#7424);
#7562=PRODUCT_DEFINITION_CONTEXT('part definition',#7651,'design');
#7563=PRODUCT_DEFINITION('PAT-006',
'PAT-006',#7592,#7562);
#7564=PRODUCT_DEFINITION('Valve body and seals','Valve body and seals',
#7593,#7562);
#7565=PRODUCT_DEFINITION('Body inlet half','Body inlet half',#7594,#7562);
#7566=PRODUCT_DEFINITION('Ball seat','Ball seat',#7595,#7562);
#7567=PRODUCT_DEFINITION('Body outlet half','Body outlet half',#7596,#7562);
#7568=PRODUCT_DEFINITION('Ball seat (1)','Ball seat (1)',#7597,#7562);
#7569=PRODUCT_DEFINITION('Split-body gasket','Split-body gasket',#7598,
#7562);
#7570=PRODUCT_DEFINITION('Stem guide','Stem guide',#7599,#7562);
#7571=PRODUCT_DEFINITION('Packing ring','Packing ring',#7600,#7562);
#7572=PRODUCT_DEFINITION('Packing retainer','Packing retainer',#7601,#7562);
#7573=PRODUCT_DEFINITION('Lever stop bridge','Lever stop bridge',#7602,
#7562);
#7574=PRODUCT_DEFINITION('Bridge spacer','Bridge spacer',#7603,#7562);
#7575=PRODUCT_DEFINITION('Bridge spacer (1)','Bridge spacer (1)',#7604,#7562);
#7576=PRODUCT_DEFINITION('Bridge spacer (2)','Bridge spacer (2)',#7605,#7562);
#7577=PRODUCT_DEFINITION('Bridge spacer (3)','Bridge spacer (3)',#7606,#7562);
#7578=PRODUCT_DEFINITION('Stop pin','Stop pin',#7607,#7562);
#7579=PRODUCT_DEFINITION('Stop pin (1)','Stop pin (1)',#7608,#7562);
#7580=PRODUCT_DEFINITION('M5x70 body screw','M5x70 body screw',#7609,#7562);
#7581=PRODUCT_DEFINITION('Flat Washer - M5','Flat Washer - M5',#7610,#7562);
#7582=PRODUCT_DEFINITION('Hex Nut - M5','Hex Nut - M5',#7611,#7562);
#7583=PRODUCT_DEFINITION(
'Hex Pipe Nipple - 1-2 Inch Tapered Pipe Thread',
'Hex Pipe Nipple - 1-2 Inch Tapered Pipe Thread',#7612,#7562);
#7584=PRODUCT_DEFINITION('Cap Screw - M4x16','Cap Screw - M4x16',#7613,
#7562);
#7585=PRODUCT_DEFINITION('Ball stem and lever','Ball stem and lever',#7614,
#7562);
#7586=PRODUCT_DEFINITION('Ported ball','Ported ball',#7615,#7562);
#7587=PRODUCT_DEFINITION('Stem','Stem',#7616,#7562);
#7588=PRODUCT_DEFINITION('Lever','Lever',#7617,#7562);
#7589=PRODUCT_DEFINITION('Lever keeper','Lever keeper',#7618,#7562);
#7590=PRODUCT_DEFINITION('Bonded grip','Bonded grip',#7619,#7562);
#7591=PRODUCT_DEFINITION('M4x10 Cap Screw','M4x10 Cap Screw',#7620,#7562);
#7592=PRODUCT_DEFINITION_FORMATION('',$,#7653);
#7593=PRODUCT_DEFINITION_FORMATION('',$,#7654);
#7594=PRODUCT_DEFINITION_FORMATION('',$,#7655);
#7595=PRODUCT_DEFINITION_FORMATION('',$,#7656);
#7596=PRODUCT_DEFINITION_FORMATION('',$,#7657);
#7597=PRODUCT_DEFINITION_FORMATION('',$,#7658);
#7598=PRODUCT_DEFINITION_FORMATION('',$,#7659);
#7599=PRODUCT_DEFINITION_FORMATION('',$,#7660);
#7600=PRODUCT_DEFINITION_FORMATION('',$,#7661);
#7601=PRODUCT_DEFINITION_FORMATION('',$,#7662);
#7602=PRODUCT_DEFINITION_FORMATION('',$,#7663);
#7603=PRODUCT_DEFINITION_FORMATION('',$,#7664);
#7604=PRODUCT_DEFINITION_FORMATION('',$,#7665);
#7605=PRODUCT_DEFINITION_FORMATION('',$,#7666);
#7606=PRODUCT_DEFINITION_FORMATION('',$,#7667);
#7607=PRODUCT_DEFINITION_FORMATION('',$,#7668);
#7608=PRODUCT_DEFINITION_FORMATION('',$,#7669);
#7609=PRODUCT_DEFINITION_FORMATION('',$,#7670);
#7610=PRODUCT_DEFINITION_FORMATION('',$,#7671);
#7611=PRODUCT_DEFINITION_FORMATION('',$,#7672);
#7612=PRODUCT_DEFINITION_FORMATION('',$,#7673);
#7613=PRODUCT_DEFINITION_FORMATION('',$,#7674);
#7614=PRODUCT_DEFINITION_FORMATION('',$,#7675);
#7615=PRODUCT_DEFINITION_FORMATION('',$,#7676);
#7616=PRODUCT_DEFINITION_FORMATION('',$,#7677);
#7617=PRODUCT_DEFINITION_FORMATION('',$,#7678);
#7618=PRODUCT_DEFINITION_FORMATION('',$,#7679);
#7619=PRODUCT_DEFINITION_FORMATION('',$,#7680);
#7620=PRODUCT_DEFINITION_FORMATION('',$,#7681);
#7621=PRODUCT_RELATED_PRODUCT_CATEGORY('PAT-006','PAT-006',(#7653));
#7622=PRODUCT_RELATED_PRODUCT_CATEGORY('Valve body and seals',
'Valve body and seals',(#7654));
#7623=PRODUCT_RELATED_PRODUCT_CATEGORY('Body inlet half',
'Body inlet half',(#7655));
#7624=PRODUCT_RELATED_PRODUCT_CATEGORY('Ball seat','Ball seat',(#7656));
#7625=PRODUCT_RELATED_PRODUCT_CATEGORY('Body outlet half',
'Body outlet half',(#7657));
#7626=PRODUCT_RELATED_PRODUCT_CATEGORY('Ball seat (1)','Ball seat (1)',
(#7658));
#7627=PRODUCT_RELATED_PRODUCT_CATEGORY('Split-body gasket',
'Split-body gasket',(#7659));
#7628=PRODUCT_RELATED_PRODUCT_CATEGORY('Stem guide','Stem guide',(#7660));
#7629=PRODUCT_RELATED_PRODUCT_CATEGORY('Packing ring','Packing ring',(#7661));
#7630=PRODUCT_RELATED_PRODUCT_CATEGORY('Packing retainer',
'Packing retainer',(#7662));
#7631=PRODUCT_RELATED_PRODUCT_CATEGORY('Lever stop bridge',
'Lever stop bridge',(#7663));
#7632=PRODUCT_RELATED_PRODUCT_CATEGORY('Bridge spacer','Bridge spacer',
(#7664));
#7633=PRODUCT_RELATED_PRODUCT_CATEGORY('Bridge spacer (1)',
'Bridge spacer (1)',(#7665));
#7634=PRODUCT_RELATED_PRODUCT_CATEGORY('Bridge spacer (2)',
'Bridge spacer (2)',(#7666));
#7635=PRODUCT_RELATED_PRODUCT_CATEGORY('Bridge spacer (3)',
'Bridge spacer (3)',(#7667));
#7636=PRODUCT_RELATED_PRODUCT_CATEGORY('Stop pin','Stop pin',(#7668));
#7637=PRODUCT_RELATED_PRODUCT_CATEGORY('Stop pin (1)','Stop pin (1)',(#7669));
#7638=PRODUCT_RELATED_PRODUCT_CATEGORY('M5x70 body screw',
'M5x70 body screw',(#7670));
#7639=PRODUCT_RELATED_PRODUCT_CATEGORY('Flat Washer - M5',
'Flat Washer - M5',(#7671));
#7640=PRODUCT_RELATED_PRODUCT_CATEGORY('Hex Nut - M5','Hex Nut - M5',(#7672));
#7641=PRODUCT_RELATED_PRODUCT_CATEGORY(
'Hex Pipe Nipple - 1-2 Inch Tapered Pipe Thread',
'Hex Pipe Nipple - 1-2 Inch Tapered Pipe Thread',(#7673));
#7642=PRODUCT_RELATED_PRODUCT_CATEGORY('Cap Screw - M4x16',
'Cap Screw - M4x16',(#7674));
#7643=PRODUCT_RELATED_PRODUCT_CATEGORY('Ball stem and lever',
'Ball stem and lever',(#7675));
#7644=PRODUCT_RELATED_PRODUCT_CATEGORY('Ported ball','Ported ball',(#7676));
#7645=PRODUCT_RELATED_PRODUCT_CATEGORY('Stem','Stem',(#7677));
#7646=PRODUCT_RELATED_PRODUCT_CATEGORY('Lever','Lever',(#7678));
#7647=PRODUCT_RELATED_PRODUCT_CATEGORY('Lever keeper','Lever keeper',(#7679));
#7648=PRODUCT_RELATED_PRODUCT_CATEGORY('Bonded grip','Bonded grip',(#7680));
#7649=PRODUCT_RELATED_PRODUCT_CATEGORY('M4x10 Cap Screw',
'M4x10 Cap Screw',(#7681));
#7650=APPLICATION_PROTOCOL_DEFINITION('international standard',
'automotive_design',2009,#7651);
#7651=APPLICATION_CONTEXT(
'Core Data for Automotive Mechanical Design Process');
#7652=PRODUCT_CONTEXT('part definition',#7651,'mechanical');
#7653=PRODUCT('PAT-006','PAT-006',
'PAT-006',(#7652));
#7654=PRODUCT('Valve body and seals','Valve body and seals',
'Valve body and seals',(#7652));
#7655=PRODUCT('Body inlet half','Body inlet half','Body inlet half',(#7652));
#7656=PRODUCT('Ball seat','Ball seat','Ball seat',(#7652));
#7657=PRODUCT('Body outlet half','Body outlet half','Body outlet half',
(#7652));
#7658=PRODUCT('Ball seat (1)','Ball seat (1)','Ball seat (1)',(#7652));
#7659=PRODUCT('Split-body gasket','Split-body gasket',
'Split-body gasket',(#7652));
#7660=PRODUCT('Stem guide','Stem guide','Stem guide',(#7652));
#7661=PRODUCT('Packing ring','Packing ring','Packing ring',(#7652));
#7662=PRODUCT('Packing retainer','Packing retainer','Packing retainer',
(#7652));
#7663=PRODUCT('Lever stop bridge','Lever stop bridge',
'Lever stop bridge',(#7652));
#7664=PRODUCT('Bridge spacer','Bridge spacer','Bridge spacer',(#7652));
#7665=PRODUCT('Bridge spacer (1)','Bridge spacer (1)','Bridge spacer (1)',(#7652));
#7666=PRODUCT('Bridge spacer (2)','Bridge spacer (2)','Bridge spacer (2)',(#7652));
#7667=PRODUCT('Bridge spacer (3)','Bridge spacer (3)','Bridge spacer (3)',(#7652));
#7668=PRODUCT('Stop pin','Stop pin','Stop pin',(#7652));
#7669=PRODUCT('Stop pin (1)','Stop pin (1)','Stop pin (1)',(#7652));
#7670=PRODUCT('M5x70 body screw','M5x70 body screw','M5x70 body screw',
(#7652));
#7671=PRODUCT('Flat Washer - M5','Flat Washer - M5','Flat Washer - M5',
(#7652));
#7672=PRODUCT('Hex Nut - M5','Hex Nut - M5','Hex Nut - M5',(#7652));
#7673=PRODUCT('Hex Pipe Nipple - 1-2 Inch Tapered Pipe Thread',
'Hex Pipe Nipple - 1-2 Inch Tapered Pipe Thread',
'Hex Pipe Nipple - 1-2 Inch Tapered Pipe Thread',(#7652));
#7674=PRODUCT('Cap Screw - M4x16','Cap Screw - M4x16',
'Cap Screw - M4x16',(#7652));
#7675=PRODUCT('Ball stem and lever','Ball stem and lever',
'Ball stem and lever',(#7652));
#7676=PRODUCT('Ported ball','Ported ball','Ported ball',(#7652));
#7677=PRODUCT('Stem','Stem','Stem',(#7652));
#7678=PRODUCT('Lever','Lever','Lever',(#7652));
#7679=PRODUCT('Lever keeper','Lever keeper','Lever keeper',(#7652));
#7680=PRODUCT('Bonded grip','Bonded grip','Bonded grip',(#7652));
#7681=PRODUCT('M4x10 Cap Screw','M4x10 Cap Screw','M4x10 Cap Screw',(#7652));
#7682=PRESENTATION_STYLE_ASSIGNMENT((#7687));
#7683=PRESENTATION_STYLE_ASSIGNMENT((#7688));
#7684=PRESENTATION_STYLE_ASSIGNMENT((#7689));
#7685=PRESENTATION_STYLE_ASSIGNMENT((#7690));
#7686=PRESENTATION_STYLE_ASSIGNMENT((#7691));
#7687=SURFACE_STYLE_USAGE(.BOTH.,#7692);
#7688=SURFACE_STYLE_USAGE(.BOTH.,#7693);
#7689=SURFACE_STYLE_USAGE(.BOTH.,#7694);
#7690=SURFACE_STYLE_USAGE(.BOTH.,#7695);
#7691=SURFACE_STYLE_USAGE(.BOTH.,#7696);
#7692=SURFACE_SIDE_STYLE('',(#7697));
#7693=SURFACE_SIDE_STYLE('',(#7698));
#7694=SURFACE_SIDE_STYLE('',(#7699));
#7695=SURFACE_SIDE_STYLE('',(#7700));
#7696=SURFACE_SIDE_STYLE('',(#7701));
#7697=SURFACE_STYLE_FILL_AREA(#7702);
#7698=SURFACE_STYLE_FILL_AREA(#7703);
#7699=SURFACE_STYLE_FILL_AREA(#7704);
#7700=SURFACE_STYLE_FILL_AREA(#7705);
#7701=SURFACE_STYLE_FILL_AREA(#7706);
#7702=FILL_AREA_STYLE('Steel - Satin',(#7707));
#7703=FILL_AREA_STYLE('CAD Library Painted - Engineering blue',(#7708));
#7704=FILL_AREA_STYLE('CAD Library Painted - Steel gray',(#7709));
#7705=FILL_AREA_STYLE('CAD Library Painted - Light blue',(#7710));
#7706=FILL_AREA_STYLE('CAD Library Painted - Graphite',(#7711));
#7707=FILL_AREA_STYLE_COLOUR('Steel - Satin',#7712);
#7708=FILL_AREA_STYLE_COLOUR('CAD Library Painted - Engineering blue',#7713);
#7709=FILL_AREA_STYLE_COLOUR('CAD Library Painted - Steel gray',#7714);
#7710=FILL_AREA_STYLE_COLOUR('CAD Library Painted - Light blue',#7715);
#7711=FILL_AREA_STYLE_COLOUR('CAD Library Painted - Graphite',#7716);
#7712=COLOUR_RGB('Steel - Satin',0.627450980392157,0.627450980392157,0.627450980392157);
#7713=COLOUR_RGB('CAD Library Painted - Engineering blue',0.12156862745098,
0.356862745098039,0.6);
#7714=COLOUR_RGB('CAD Library Painted - Steel gray',0.592156862745098,0.631372549019608,
0.67843137254902);
#7715=COLOUR_RGB('CAD Library Painted - Light blue',0.286274509803922,0.552941176470588,
0.780392156862745);
#7716=COLOUR_RGB('CAD Library Painted - Graphite',0.168627450980392,0.192156862745098,
0.231372549019608);
#7717=COLOUR_RGB('Dark Blue',0.08,0.2,0.34);
#7718=FILL_AREA_STYLE_COLOUR('',#7717);
#7719=FILL_AREA_STYLE('',(#7718));
#7720=SURFACE_STYLE_FILL_AREA(#7719);
#7721=SURFACE_SIDE_STYLE('',(#7720));
#7722=SURFACE_STYLE_USAGE(.BOTH.,#7721);
#7723=PRESENTATION_STYLE_ASSIGNMENT((#7722));
#7724=COLOUR_RGB('Light Blue',0.38,0.62,0.78);
#7725=FILL_AREA_STYLE_COLOUR('',#7724);
#7726=FILL_AREA_STYLE('',(#7725));
#7727=SURFACE_STYLE_FILL_AREA(#7726);
#7728=SURFACE_SIDE_STYLE('',(#7727));
#7729=SURFACE_STYLE_USAGE(.BOTH.,#7728);
#7730=PRESENTATION_STYLE_ASSIGNMENT((#7729));
#7731=COLOUR_RGB('Sky Blue',0.24,0.69,0.87);
#7732=FILL_AREA_STYLE_COLOUR('',#7731);
#7733=FILL_AREA_STYLE('',(#7732));
#7734=SURFACE_STYLE_FILL_AREA(#7733);
#7735=SURFACE_SIDE_STYLE('',(#7734));
#7736=SURFACE_STYLE_USAGE(.BOTH.,#7735);
#7737=PRESENTATION_STYLE_ASSIGNMENT((#7736));
#7738=COLOUR_RGB('Grey',0.48,0.52,0.57);
#7739=FILL_AREA_STYLE_COLOUR('',#7738);
#7740=FILL_AREA_STYLE('',(#7739));
#7741=SURFACE_STYLE_FILL_AREA(#7740);
#7742=SURFACE_SIDE_STYLE('',(#7741));
#7743=SURFACE_STYLE_USAGE(.BOTH.,#7742);
#7744=PRESENTATION_STYLE_ASSIGNMENT((#7743));
#7745=COLOUR_RGB('Black',0.12,0.14,0.17);
#7746=FILL_AREA_STYLE_COLOUR('',#7745);
#7747=FILL_AREA_STYLE('',(#7746));
#7748=SURFACE_STYLE_FILL_AREA(#7747);
#7749=SURFACE_SIDE_STYLE('',(#7748));
#7750=SURFACE_STYLE_USAGE(.BOTH.,#7749);
#7751=PRESENTATION_STYLE_ASSIGNMENT((#7750));
#7752=COLOUR_RGB('Off White',0.89,0.88,0.83);
#7753=FILL_AREA_STYLE_COLOUR('',#7752);
#7754=FILL_AREA_STYLE('',(#7753));
#7755=SURFACE_STYLE_FILL_AREA(#7754);
#7756=SURFACE_SIDE_STYLE('',(#7755));
#7757=SURFACE_STYLE_USAGE(.BOTH.,#7756);
#7758=PRESENTATION_STYLE_ASSIGNMENT((#7757));
ENDSEC;
END-ISO-10303-21;
